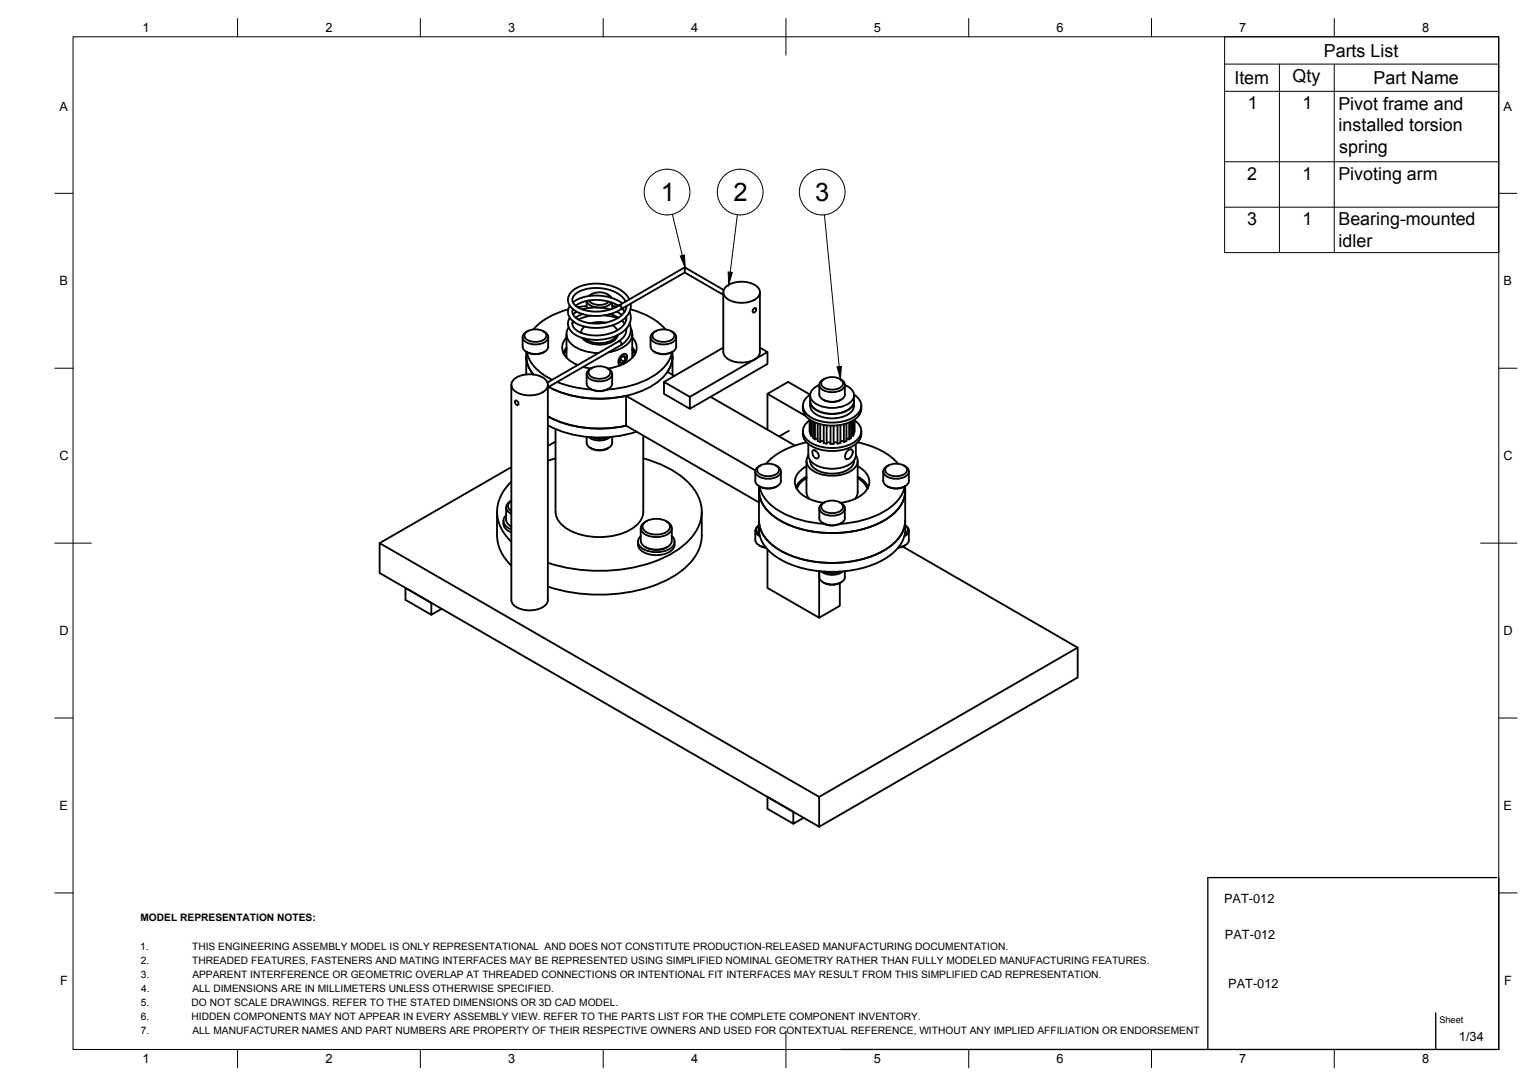
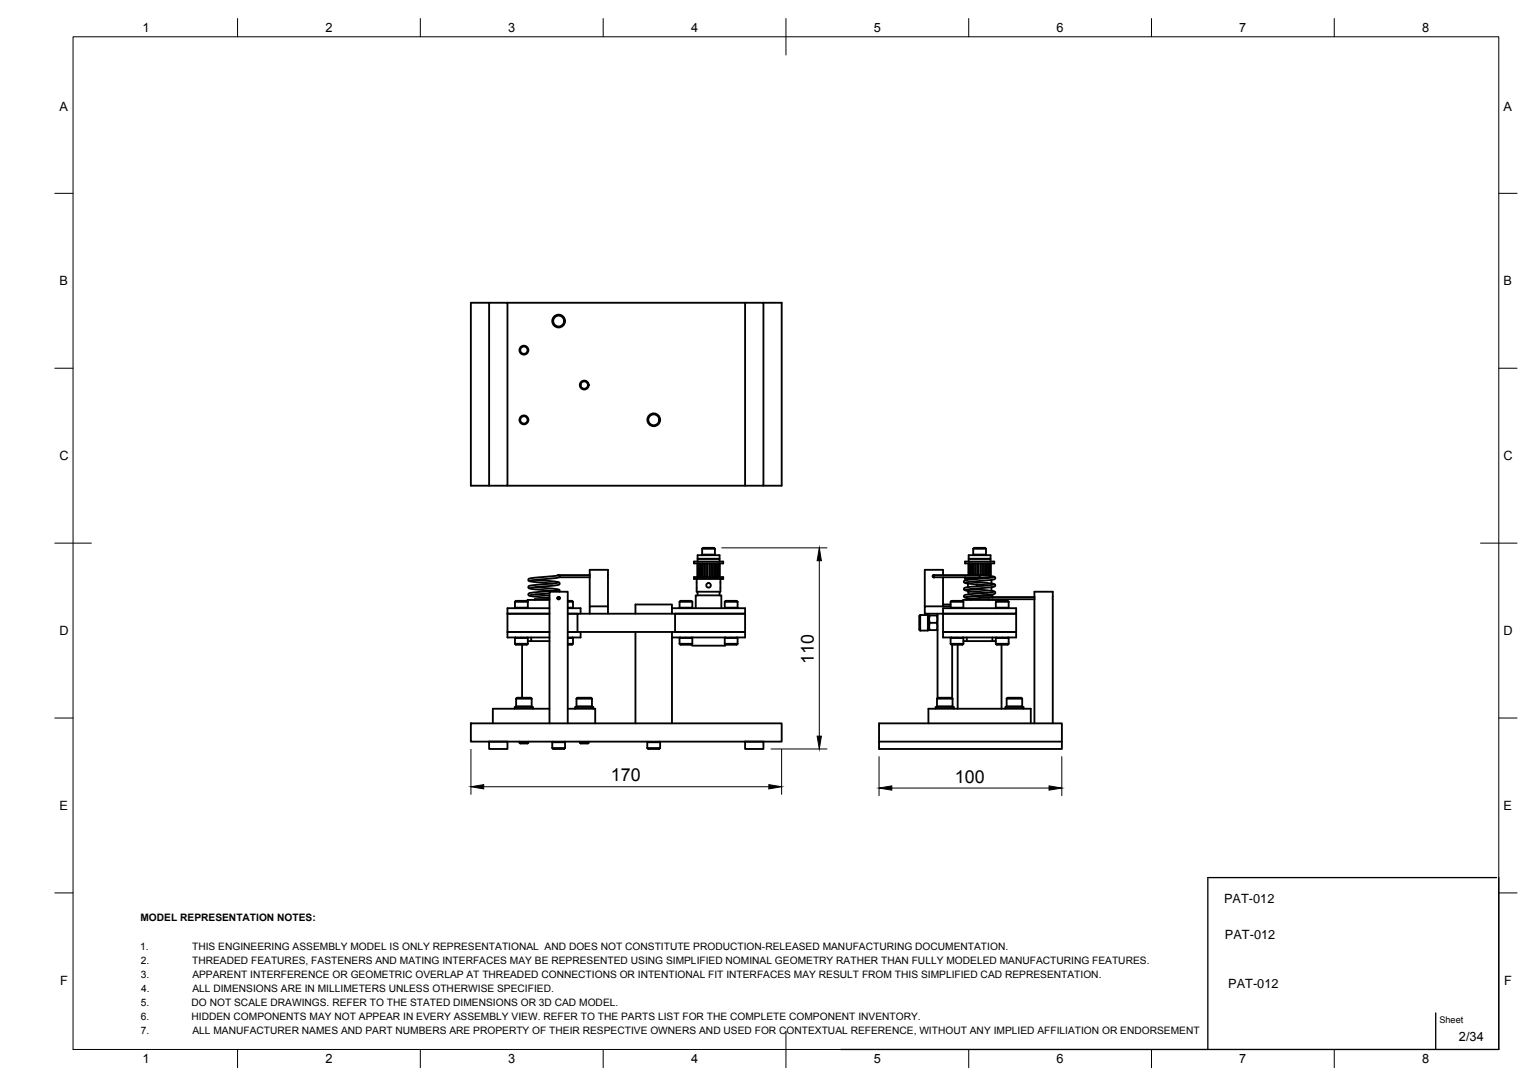
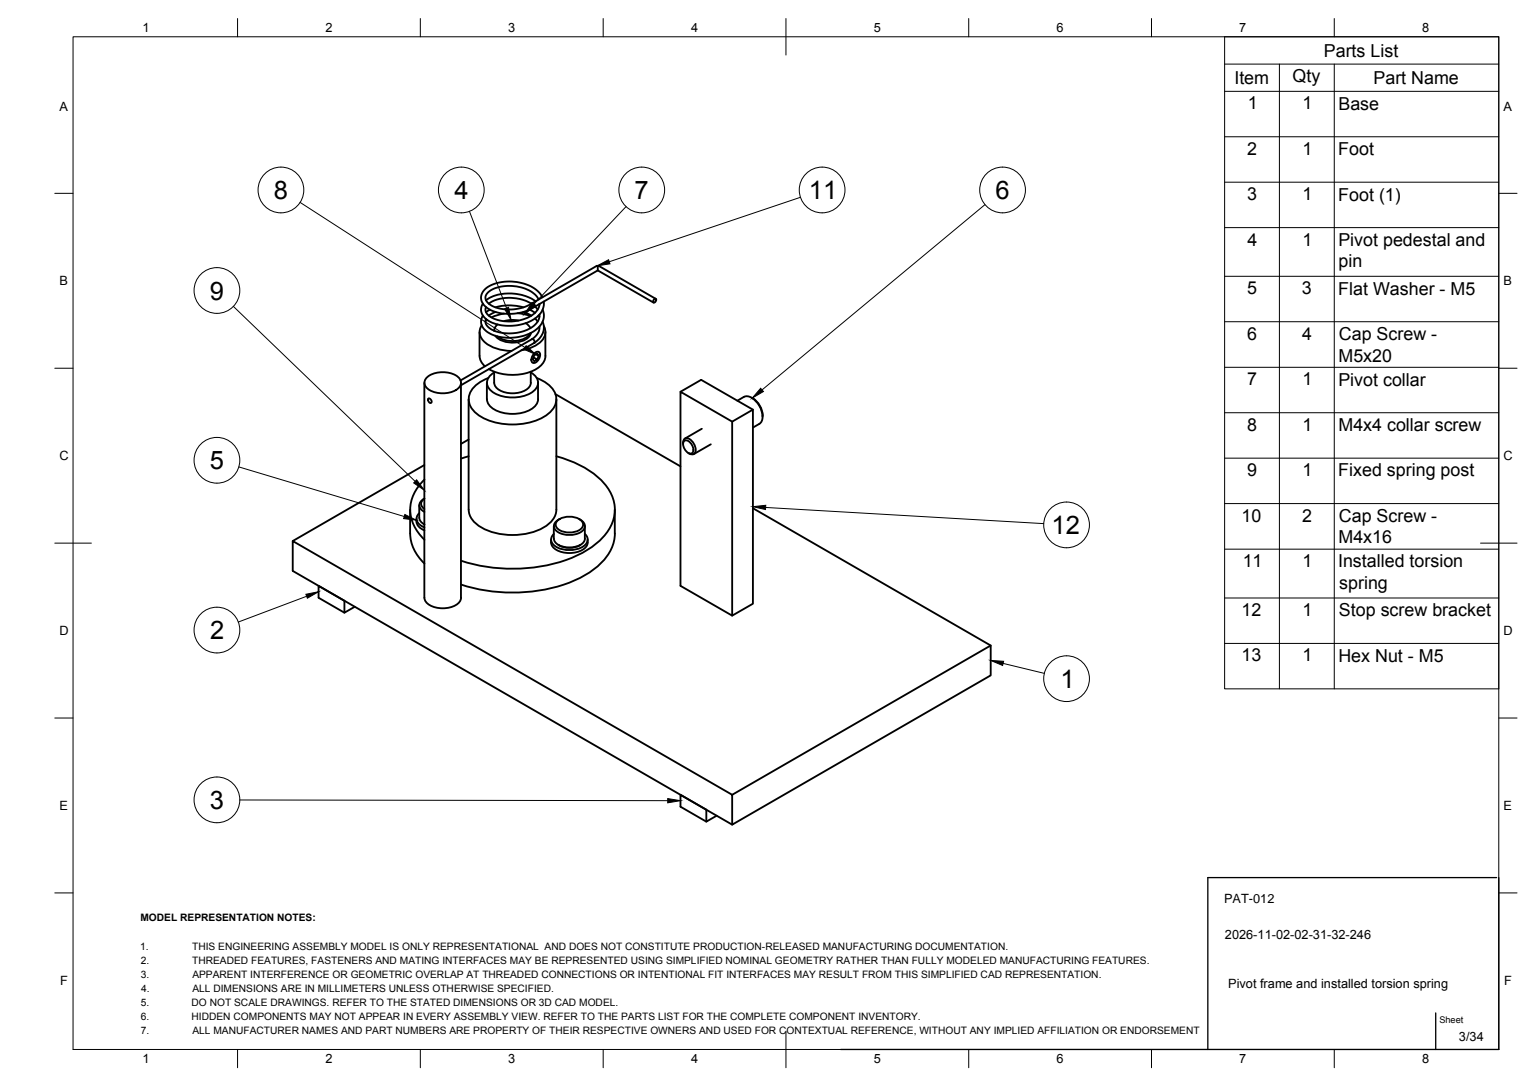
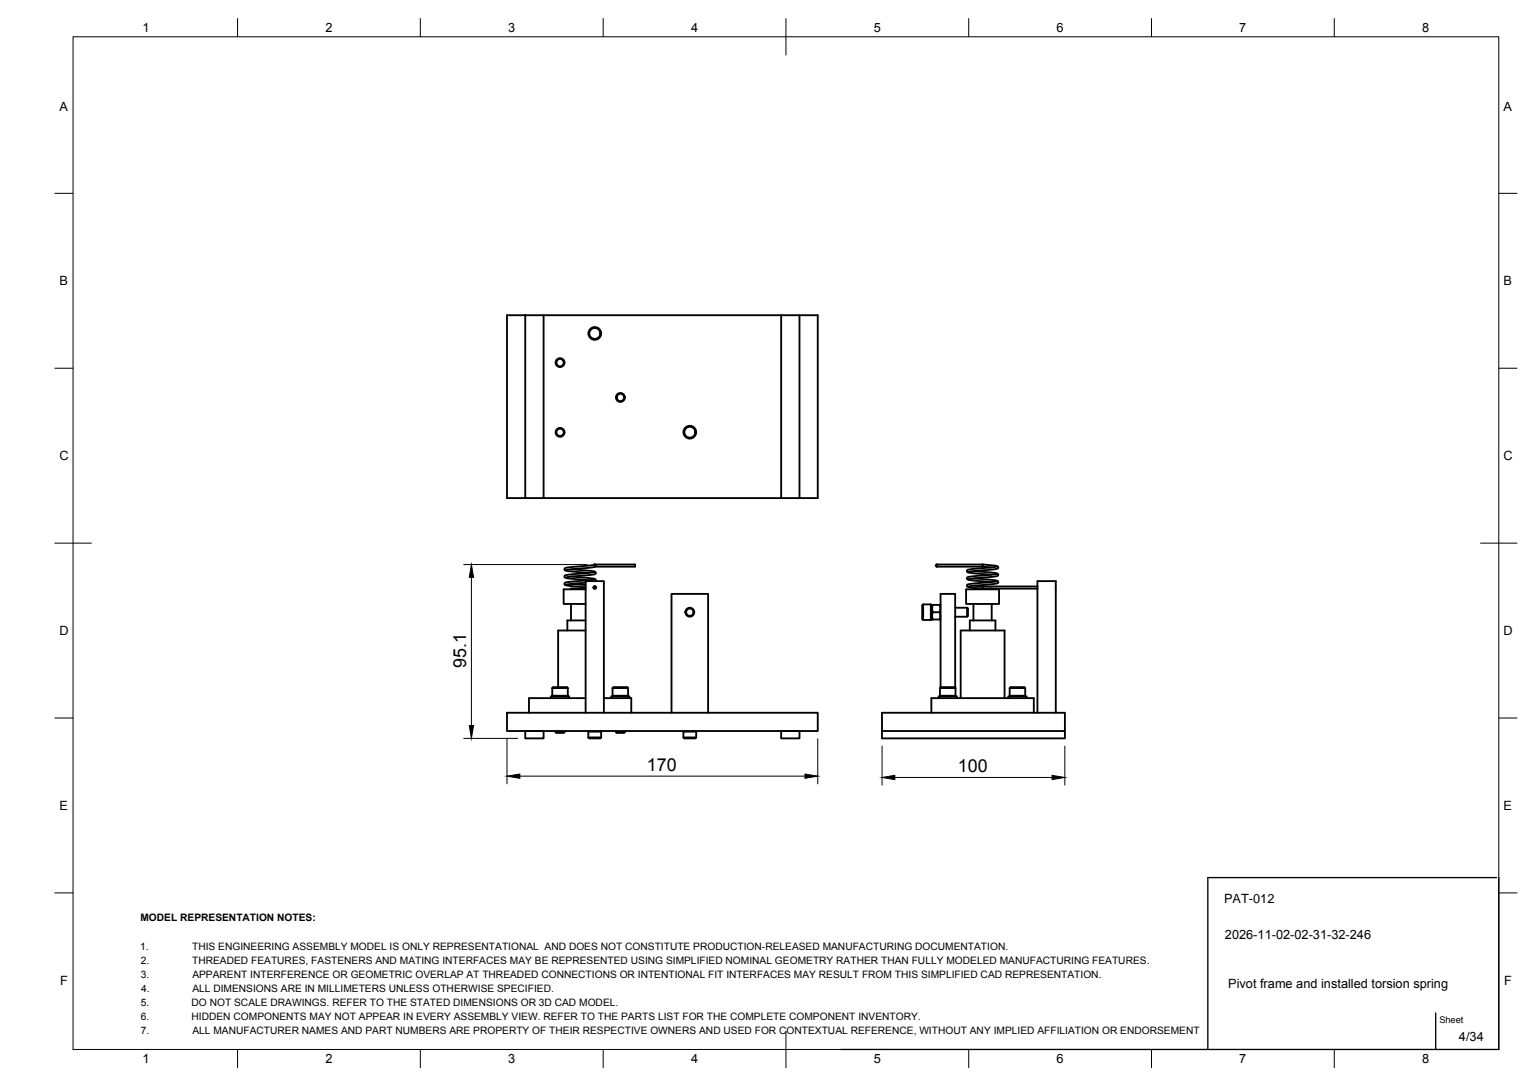
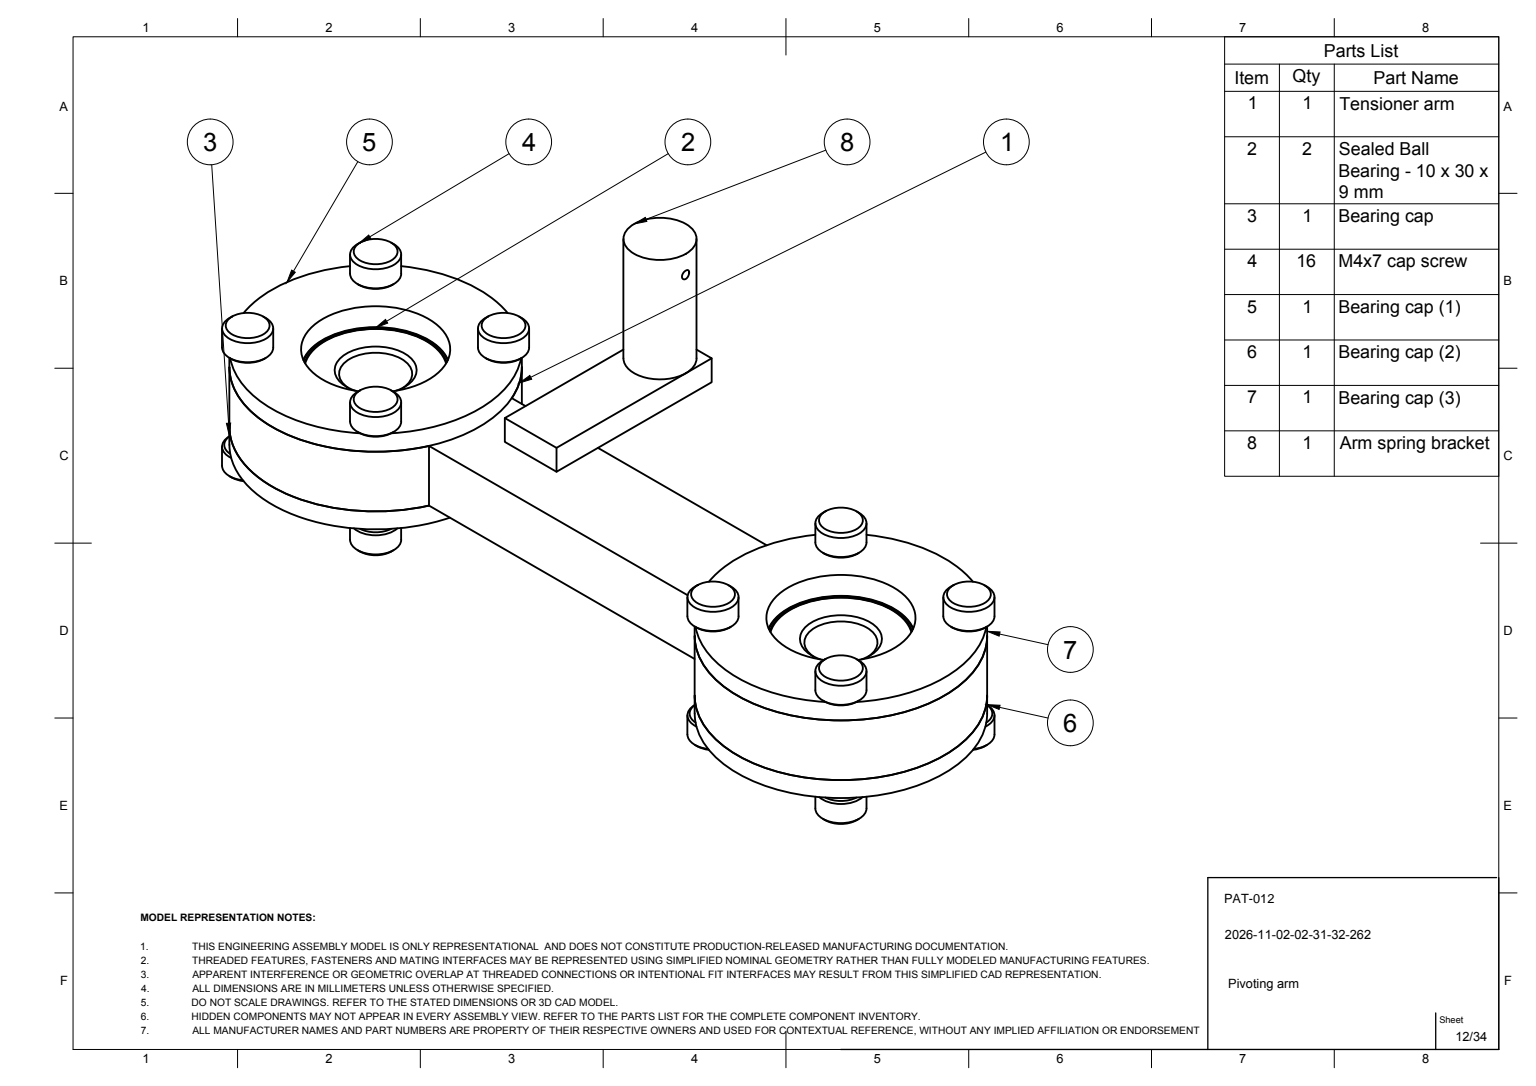
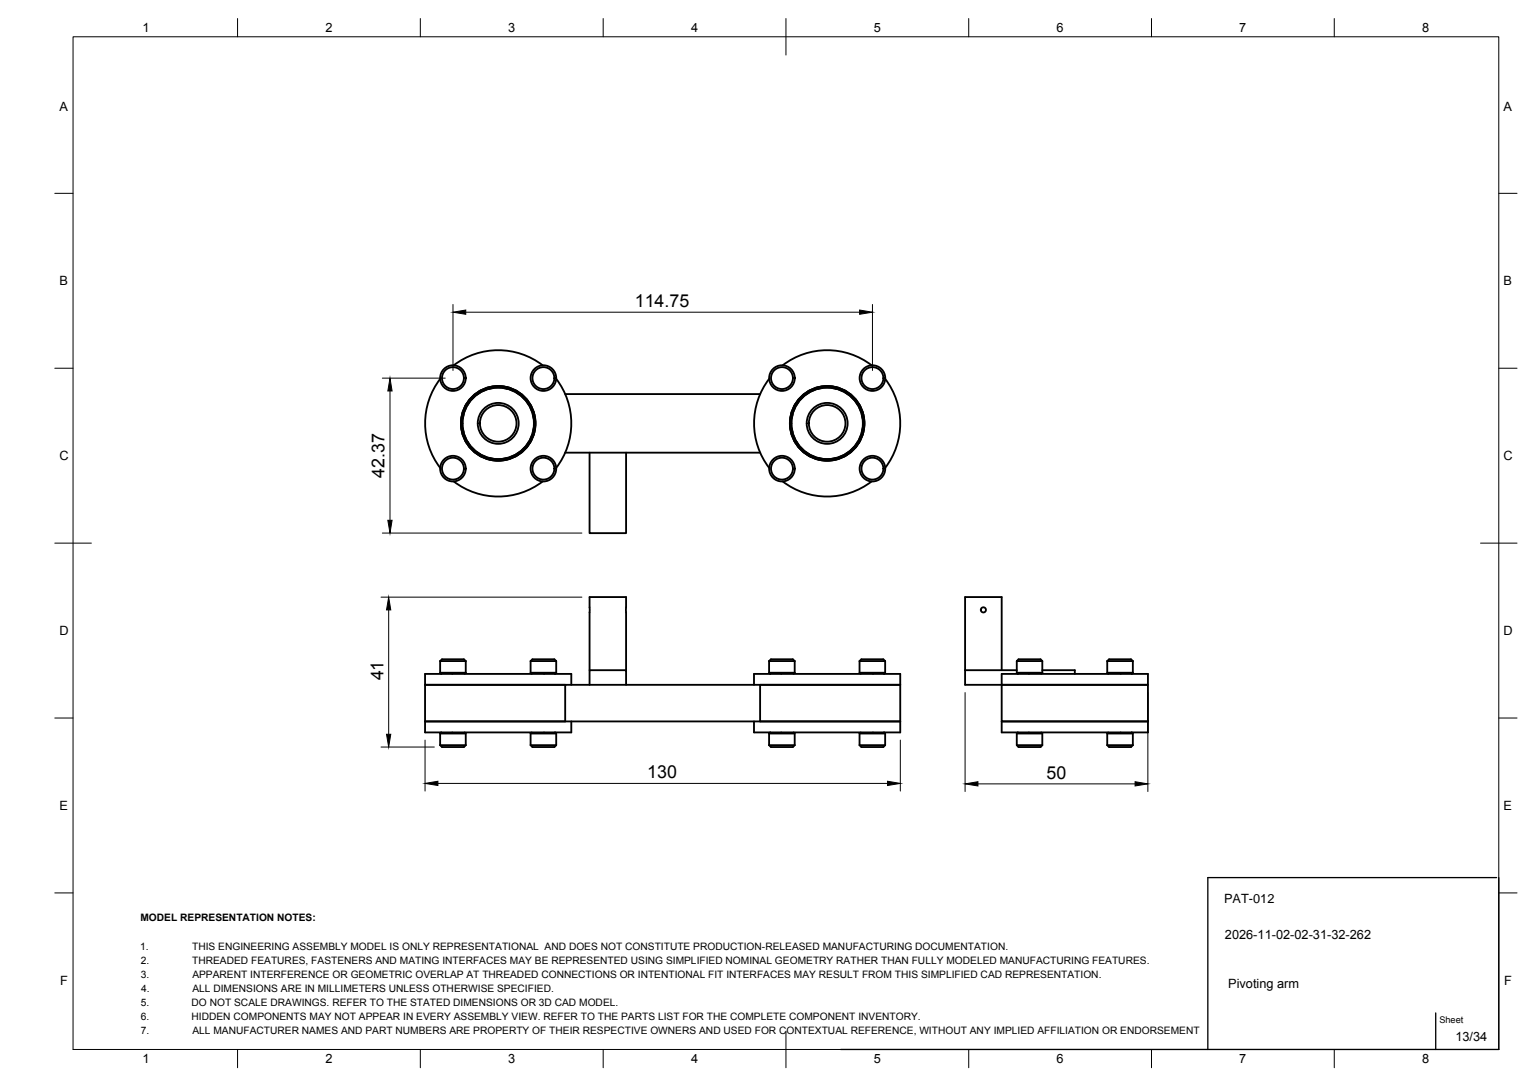
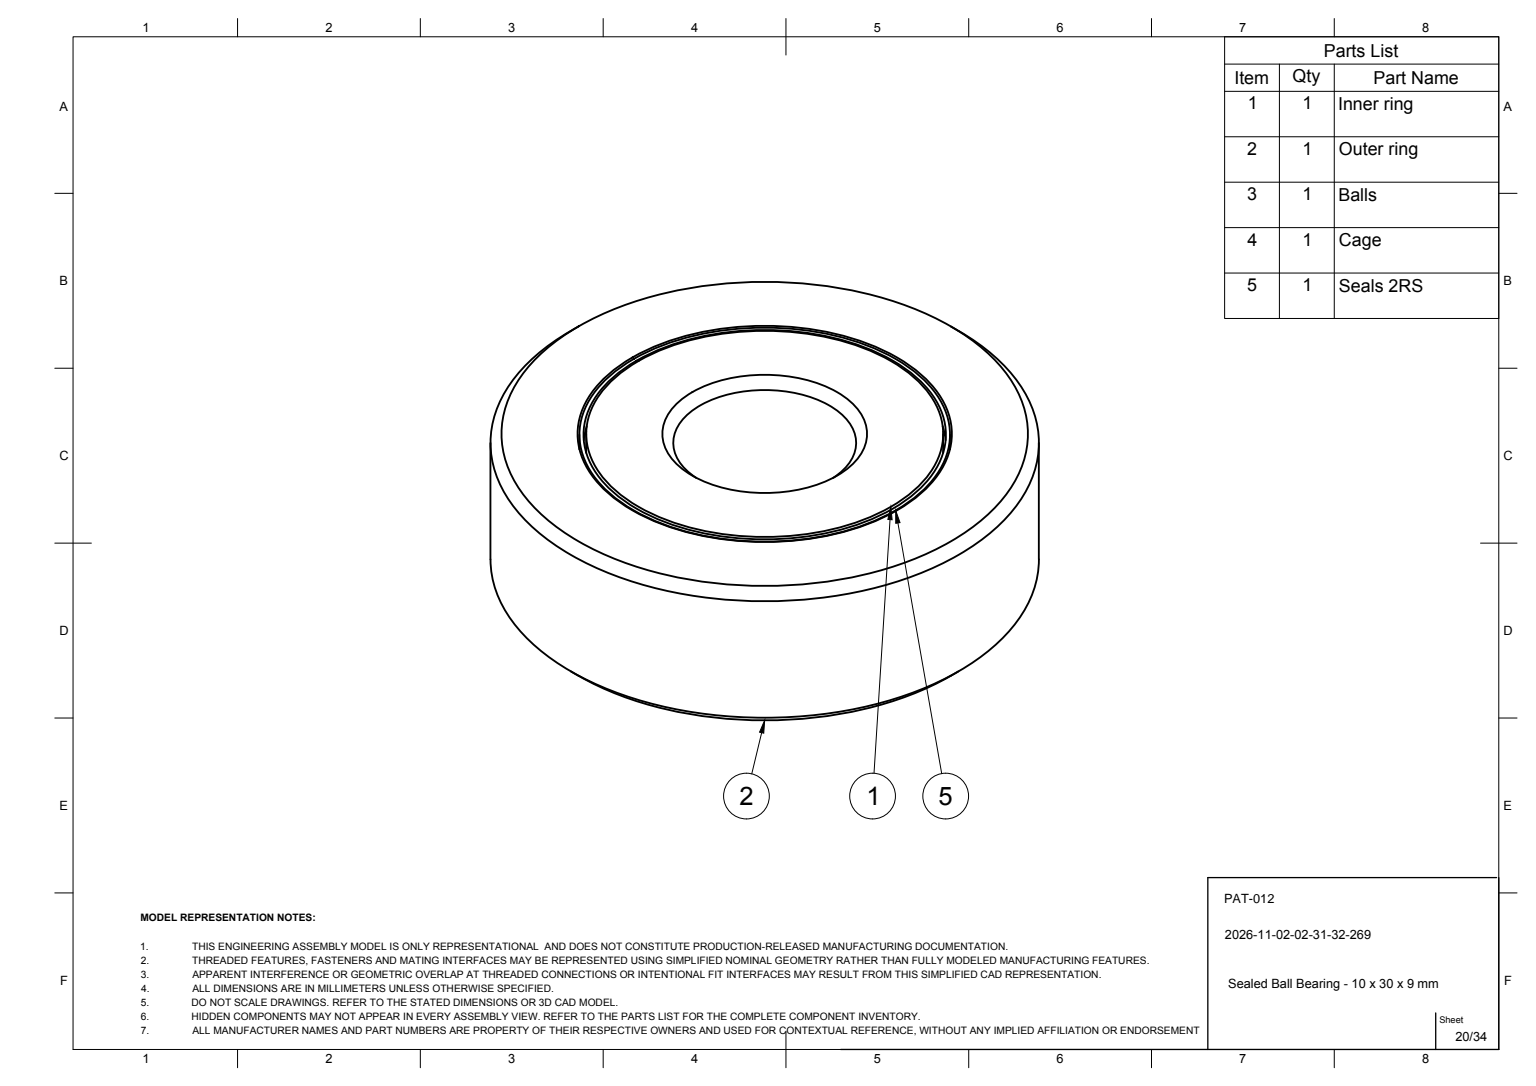
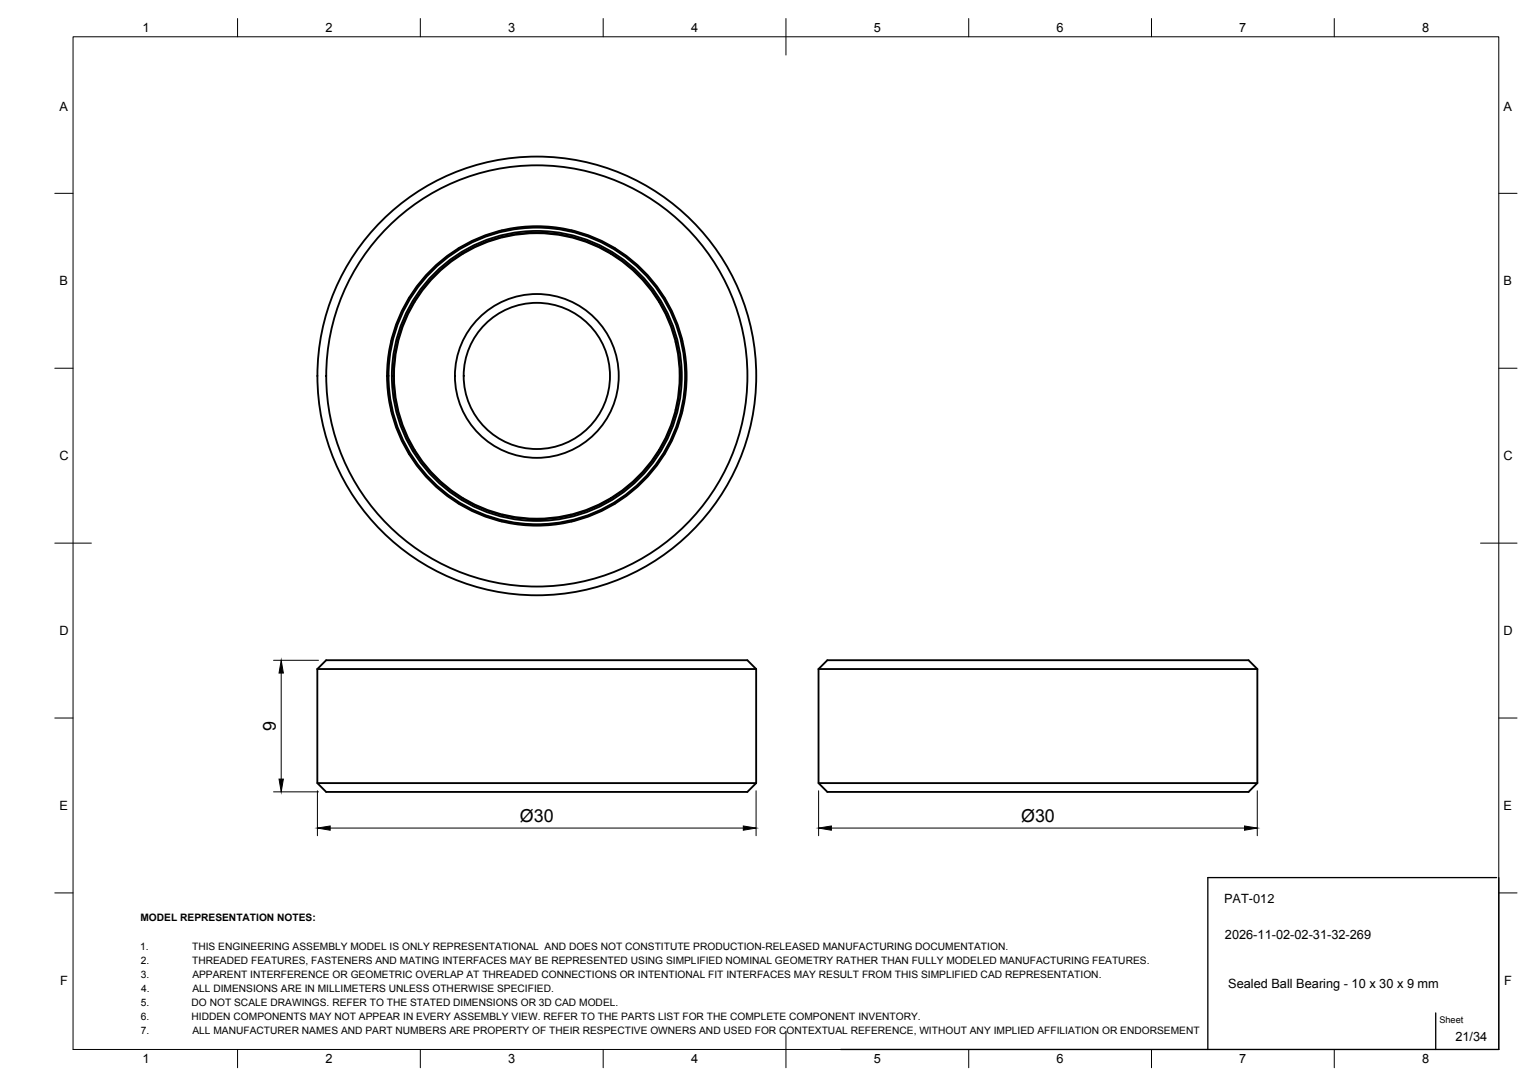
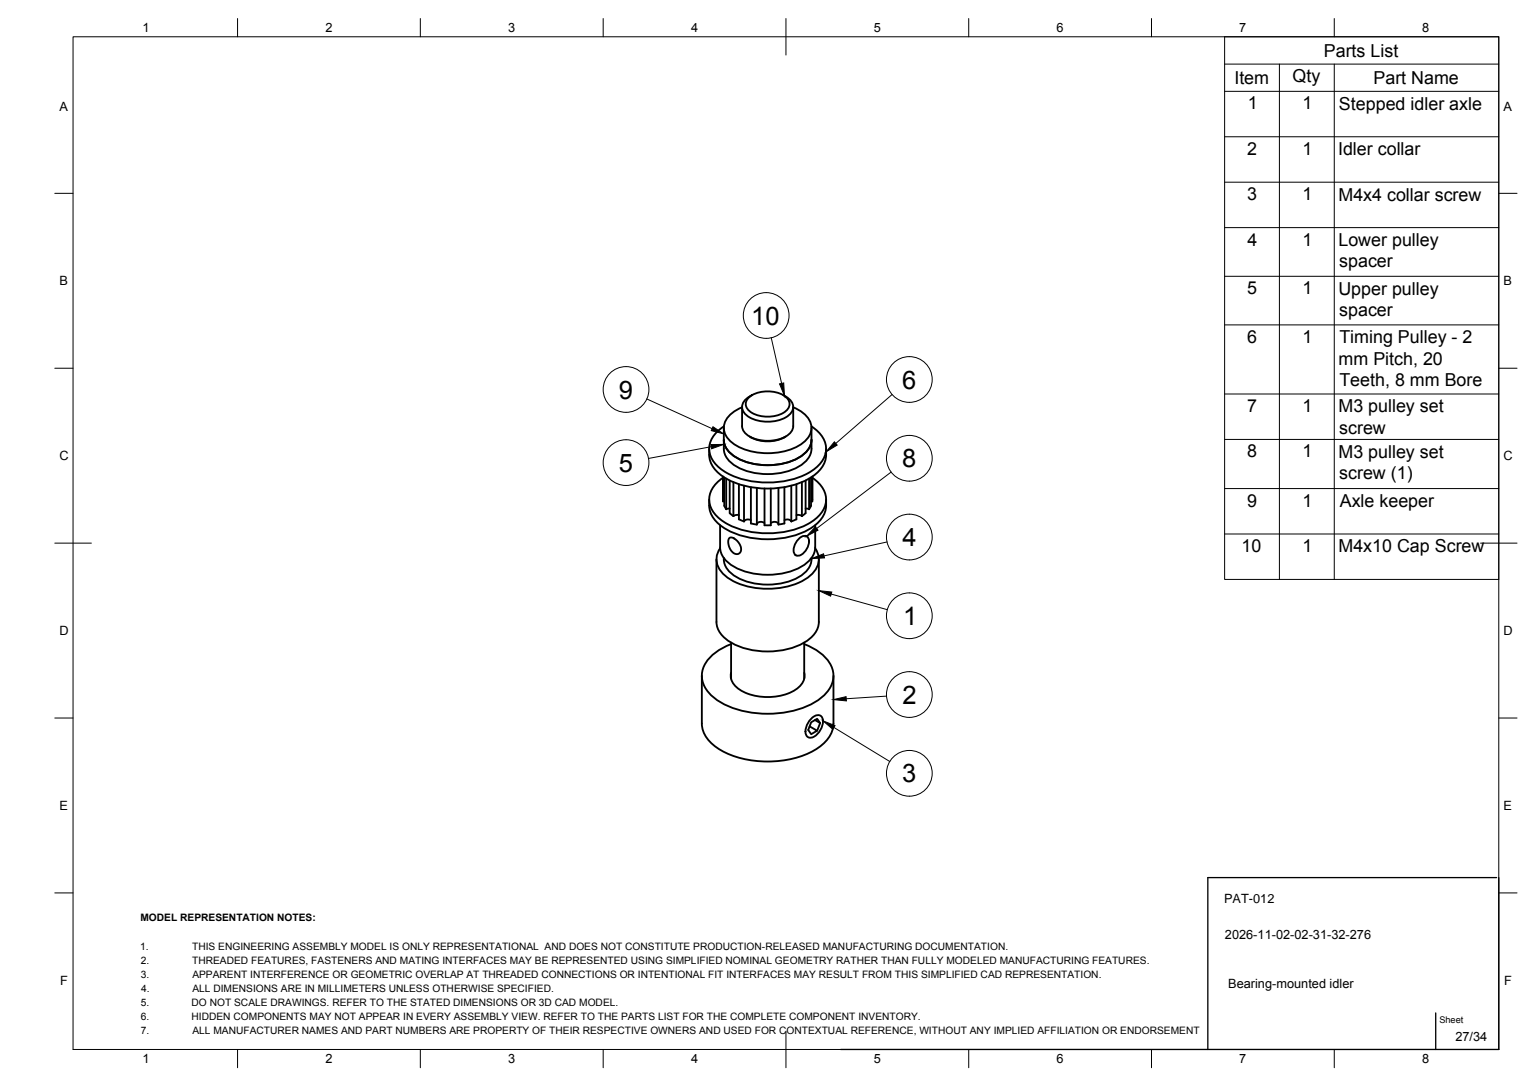
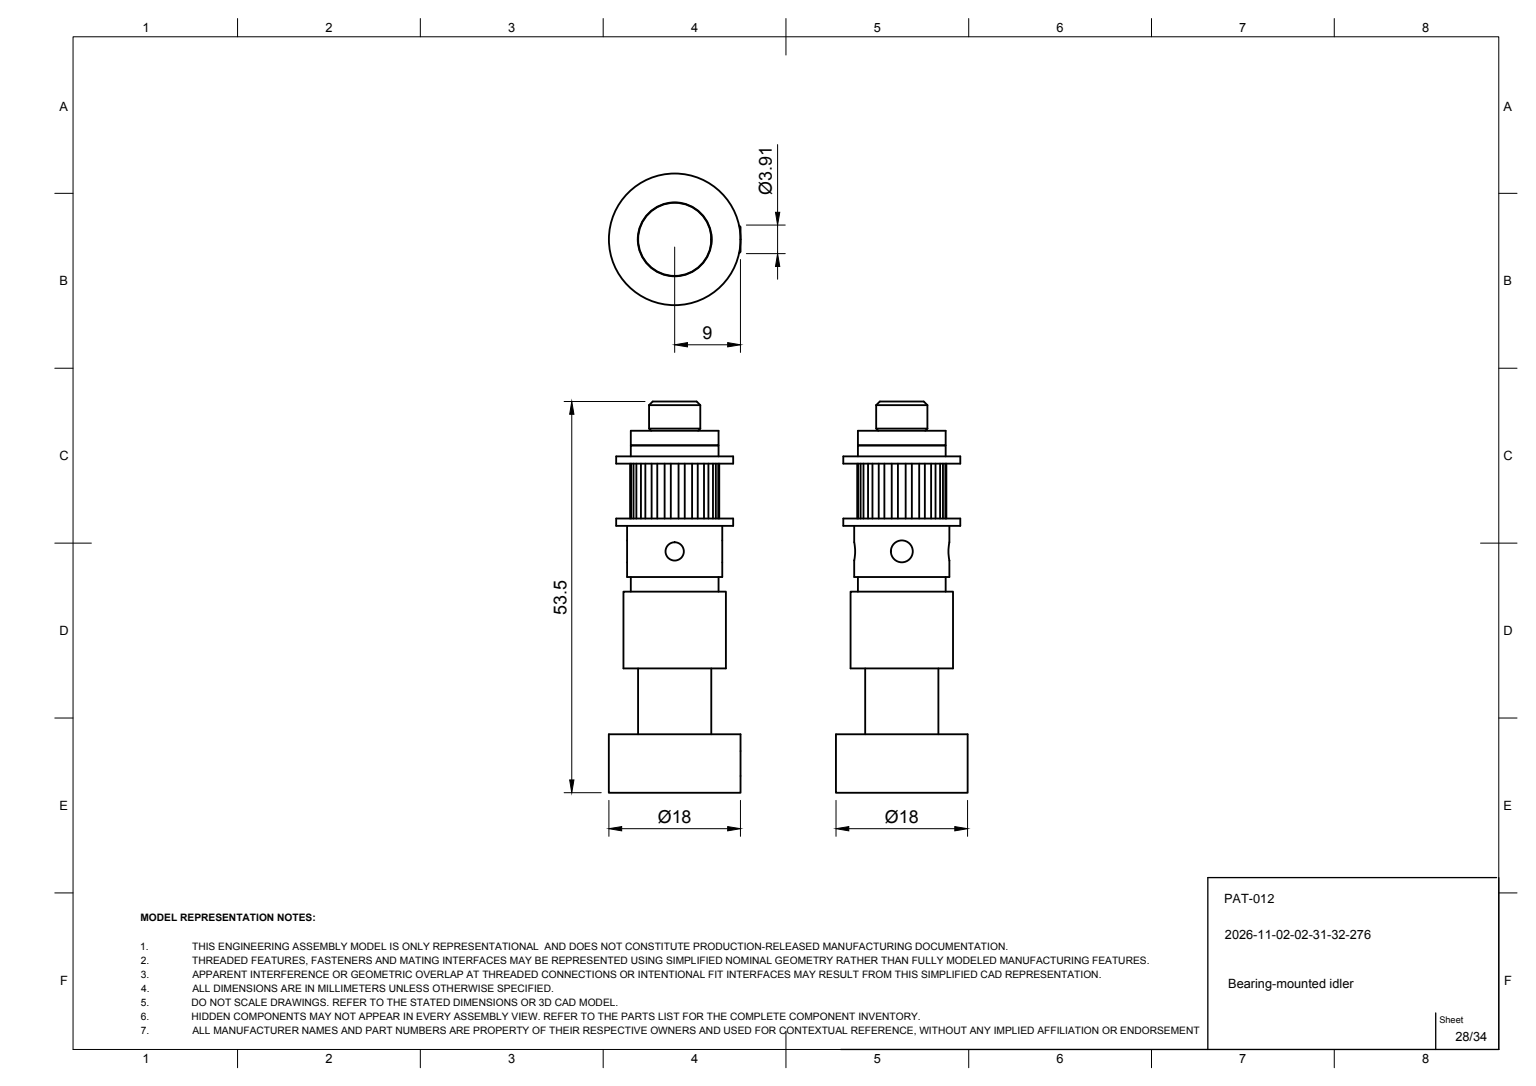
ISO-10303-21;
HEADER;
/* Generated by software containing ST-Developer
 * from STEP Tools, Inc. (www.steptools.com) 
 */

FILE_DESCRIPTION(
/* description */ ('Belt tensioner idler arm'),
/* implementation_level */ '2;1');

FILE_NAME(
/* name */ 'PAT-012',
/* time_stamp */ '2026-10-28T03:22:15-07:00',
/* author */ (''),
/* organization */ (''),
/* preprocessor_version */ 'ST-DEVELOPER v20.2',
/* originating_system */ 'Autodesk Translation Framework v15.17.0.0',
/* authorisation */ '');

FILE_SCHEMA (('AUTOMOTIVE_DESIGN { 1 0 10303 214 3 1 1 }'));
ENDSEC;

DATA;
#10=MECHANICAL_DESIGN_GEOMETRIC_PRESENTATION_REPRESENTATION('',(#447,#448,
#449,#450,#451,#452,#453,#454,#455,#456,#457,#458,#459,#460,#461,#462,#463,
#464,#465,#466,#467,#468,#469,#470,#471,#472,#473,#474,#475,#476,#477,#478,
#479,#480,#481,#482,#483,#484,#485,#486,#487,#488),#12779);
#11=ITEM_DEFINED_TRANSFORMATION($,$,#6967,#7095);
#12=ITEM_DEFINED_TRANSFORMATION($,$,#6987,#7096);
#13=ITEM_DEFINED_TRANSFORMATION($,$,#7007,#7097);
#14=ITEM_DEFINED_TRANSFORMATION($,$,#7024,#7098);
#15=ITEM_DEFINED_TRANSFORMATION($,$,#7078,#7099);
#16=ITEM_DEFINED_TRANSFORMATION($,$,#6809,#7124);
#17=ITEM_DEFINED_TRANSFORMATION($,$,#6850,#7125);
#18=ITEM_DEFINED_TRANSFORMATION($,$,#6875,#7126);
#19=ITEM_DEFINED_TRANSFORMATION($,$,#6900,#7127);
#20=ITEM_DEFINED_TRANSFORMATION($,$,#6925,#7128);
#21=ITEM_DEFINED_TRANSFORMATION($,$,#6950,#7129);
#22=ITEM_DEFINED_TRANSFORMATION($,$,#6966,#7130);
#23=ITEM_DEFINED_TRANSFORMATION($,$,#7100,#7131);
#24=ITEM_DEFINED_TRANSFORMATION($,$,#7100,#7132);
#25=ITEM_DEFINED_TRANSFORMATION($,$,#7100,#7133);
#26=ITEM_DEFINED_TRANSFORMATION($,$,#7100,#7134);
#27=ITEM_DEFINED_TRANSFORMATION($,$,#7100,#7135);
#28=ITEM_DEFINED_TRANSFORMATION($,$,#7100,#7136);
#29=ITEM_DEFINED_TRANSFORMATION($,$,#7100,#7137);
#30=ITEM_DEFINED_TRANSFORMATION($,$,#7100,#7138);
#31=ITEM_DEFINED_TRANSFORMATION($,$,#6966,#7139);
#32=ITEM_DEFINED_TRANSFORMATION($,$,#7100,#7140);
#33=ITEM_DEFINED_TRANSFORMATION($,$,#7100,#7141);
#34=ITEM_DEFINED_TRANSFORMATION($,$,#7100,#7142);
#35=ITEM_DEFINED_TRANSFORMATION($,$,#7100,#7143);
#36=ITEM_DEFINED_TRANSFORMATION($,$,#7100,#7144);
#37=ITEM_DEFINED_TRANSFORMATION($,$,#7100,#7145);
#38=ITEM_DEFINED_TRANSFORMATION($,$,#7100,#7146);
#39=ITEM_DEFINED_TRANSFORMATION($,$,#7100,#7147);
#40=ITEM_DEFINED_TRANSFORMATION($,$,#6604,#7235);
#41=ITEM_DEFINED_TRANSFORMATION($,$,#6626,#7236);
#42=ITEM_DEFINED_TRANSFORMATION($,$,#6633,#7237);
#43=ITEM_DEFINED_TRANSFORMATION($,$,#6640,#7238);
#44=ITEM_DEFINED_TRANSFORMATION($,$,#6667,#7239);
#45=ITEM_DEFINED_TRANSFORMATION($,$,#6681,#7240);
#46=ITEM_DEFINED_TRANSFORMATION($,$,#6692,#7241);
#47=ITEM_DEFINED_TRANSFORMATION($,$,#6715,#7242);
#48=ITEM_DEFINED_TRANSFORMATION($,$,#6729,#7243);
#49=ITEM_DEFINED_TRANSFORMATION($,$,#6740,#7244);
#50=ITEM_DEFINED_TRANSFORMATION($,$,#6729,#7245);
#51=ITEM_DEFINED_TRANSFORMATION($,$,#6740,#7246);
#52=ITEM_DEFINED_TRANSFORMATION($,$,#6729,#7247);
#53=ITEM_DEFINED_TRANSFORMATION($,$,#6740,#7248);
#54=ITEM_DEFINED_TRANSFORMATION($,$,#7220,#7249);
#55=ITEM_DEFINED_TRANSFORMATION($,$,#6782,#7250);
#56=ITEM_DEFINED_TRANSFORMATION($,$,#6740,#7251);
#57=ITEM_DEFINED_TRANSFORMATION($,$,#6766,#7252);
#58=ITEM_DEFINED_TRANSFORMATION($,$,#6782,#7253);
#59=ITEM_DEFINED_TRANSFORMATION($,$,#7149,#7420);
#60=ITEM_DEFINED_TRANSFORMATION($,$,#7167,#7421);
#61=ITEM_DEFINED_TRANSFORMATION($,$,#7181,#7422);
#62=ITEM_DEFINED_TRANSFORMATION($,$,#7190,#7423);
#63=ITEM_DEFINED_TRANSFORMATION($,$,#7199,#7424);
#64=ITEM_DEFINED_TRANSFORMATION($,$,#7205,#7425);
#65=ITEM_DEFINED_TRANSFORMATION($,$,#7211,#7426);
#66=ITEM_DEFINED_TRANSFORMATION($,$,#7220,#7427);
#67=ITEM_DEFINED_TRANSFORMATION($,$,#7254,#7428);
#68=ITEM_DEFINED_TRANSFORMATION($,$,#7396,#7429);
#69=ITEM_DEFINED_TRANSFORMATION($,$,#6603,#7430);
#70=ITEM_DEFINED_TRANSFORMATION($,$,#6808,#7431);
#71=ITEM_DEFINED_TRANSFORMATION($,$,#7148,#7432);
#72=(
REPRESENTATION_RELATIONSHIP($,$,#12945,#12944)
REPRESENTATION_RELATIONSHIP_WITH_TRANSFORMATION(#11)
SHAPE_REPRESENTATION_RELATIONSHIP()
);
#73=(
REPRESENTATION_RELATIONSHIP($,$,#12946,#12944)
REPRESENTATION_RELATIONSHIP_WITH_TRANSFORMATION(#12)
SHAPE_REPRESENTATION_RELATIONSHIP()
);
#74=(
REPRESENTATION_RELATIONSHIP($,$,#12947,#12944)
REPRESENTATION_RELATIONSHIP_WITH_TRANSFORMATION(#13)
SHAPE_REPRESENTATION_RELATIONSHIP()
);
#75=(
REPRESENTATION_RELATIONSHIP($,$,#12948,#12944)
REPRESENTATION_RELATIONSHIP_WITH_TRANSFORMATION(#14)
SHAPE_REPRESENTATION_RELATIONSHIP()
);
#76=(
REPRESENTATION_RELATIONSHIP($,$,#12949,#12944)
REPRESENTATION_RELATIONSHIP_WITH_TRANSFORMATION(#15)
SHAPE_REPRESENTATION_RELATIONSHIP()
);
#77=(
REPRESENTATION_RELATIONSHIP($,$,#12938,#12937)
REPRESENTATION_RELATIONSHIP_WITH_TRANSFORMATION(#16)
SHAPE_REPRESENTATION_RELATIONSHIP()
);
#78=(
REPRESENTATION_RELATIONSHIP($,$,#12939,#12937)
REPRESENTATION_RELATIONSHIP_WITH_TRANSFORMATION(#17)
SHAPE_REPRESENTATION_RELATIONSHIP()
);
#79=(
REPRESENTATION_RELATIONSHIP($,$,#12940,#12937)
REPRESENTATION_RELATIONSHIP_WITH_TRANSFORMATION(#18)
SHAPE_REPRESENTATION_RELATIONSHIP()
);
#80=(
REPRESENTATION_RELATIONSHIP($,$,#12941,#12937)
REPRESENTATION_RELATIONSHIP_WITH_TRANSFORMATION(#19)
SHAPE_REPRESENTATION_RELATIONSHIP()
);
#81=(
REPRESENTATION_RELATIONSHIP($,$,#12942,#12937)
REPRESENTATION_RELATIONSHIP_WITH_TRANSFORMATION(#20)
SHAPE_REPRESENTATION_RELATIONSHIP()
);
#82=(
REPRESENTATION_RELATIONSHIP($,$,#12943,#12937)
REPRESENTATION_RELATIONSHIP_WITH_TRANSFORMATION(#21)
SHAPE_REPRESENTATION_RELATIONSHIP()
);
#83=(
REPRESENTATION_RELATIONSHIP($,$,#12944,#12937)
REPRESENTATION_RELATIONSHIP_WITH_TRANSFORMATION(#22)
SHAPE_REPRESENTATION_RELATIONSHIP()
);
#84=(
REPRESENTATION_RELATIONSHIP($,$,#12950,#12937)
REPRESENTATION_RELATIONSHIP_WITH_TRANSFORMATION(#23)
SHAPE_REPRESENTATION_RELATIONSHIP()
);
#85=(
REPRESENTATION_RELATIONSHIP($,$,#12950,#12937)
REPRESENTATION_RELATIONSHIP_WITH_TRANSFORMATION(#24)
SHAPE_REPRESENTATION_RELATIONSHIP()
);
#86=(
REPRESENTATION_RELATIONSHIP($,$,#12950,#12937)
REPRESENTATION_RELATIONSHIP_WITH_TRANSFORMATION(#25)
SHAPE_REPRESENTATION_RELATIONSHIP()
);
#87=(
REPRESENTATION_RELATIONSHIP($,$,#12950,#12937)
REPRESENTATION_RELATIONSHIP_WITH_TRANSFORMATION(#26)
SHAPE_REPRESENTATION_RELATIONSHIP()
);
#88=(
REPRESENTATION_RELATIONSHIP($,$,#12950,#12937)
REPRESENTATION_RELATIONSHIP_WITH_TRANSFORMATION(#27)
SHAPE_REPRESENTATION_RELATIONSHIP()
);
#89=(
REPRESENTATION_RELATIONSHIP($,$,#12950,#12937)
REPRESENTATION_RELATIONSHIP_WITH_TRANSFORMATION(#28)
SHAPE_REPRESENTATION_RELATIONSHIP()
);
#90=(
REPRESENTATION_RELATIONSHIP($,$,#12950,#12937)
REPRESENTATION_RELATIONSHIP_WITH_TRANSFORMATION(#29)
SHAPE_REPRESENTATION_RELATIONSHIP()
);
#91=(
REPRESENTATION_RELATIONSHIP($,$,#12950,#12937)
REPRESENTATION_RELATIONSHIP_WITH_TRANSFORMATION(#30)
SHAPE_REPRESENTATION_RELATIONSHIP()
);
#92=(
REPRESENTATION_RELATIONSHIP($,$,#12944,#12937)
REPRESENTATION_RELATIONSHIP_WITH_TRANSFORMATION(#31)
SHAPE_REPRESENTATION_RELATIONSHIP()
);
#93=(
REPRESENTATION_RELATIONSHIP($,$,#12950,#12937)
REPRESENTATION_RELATIONSHIP_WITH_TRANSFORMATION(#32)
SHAPE_REPRESENTATION_RELATIONSHIP()
);
#94=(
REPRESENTATION_RELATIONSHIP($,$,#12950,#12937)
REPRESENTATION_RELATIONSHIP_WITH_TRANSFORMATION(#33)
SHAPE_REPRESENTATION_RELATIONSHIP()
);
#95=(
REPRESENTATION_RELATIONSHIP($,$,#12950,#12937)
REPRESENTATION_RELATIONSHIP_WITH_TRANSFORMATION(#34)
SHAPE_REPRESENTATION_RELATIONSHIP()
);
#96=(
REPRESENTATION_RELATIONSHIP($,$,#12950,#12937)
REPRESENTATION_RELATIONSHIP_WITH_TRANSFORMATION(#35)
SHAPE_REPRESENTATION_RELATIONSHIP()
);
#97=(
REPRESENTATION_RELATIONSHIP($,$,#12950,#12937)
REPRESENTATION_RELATIONSHIP_WITH_TRANSFORMATION(#36)
SHAPE_REPRESENTATION_RELATIONSHIP()
);
#98=(
REPRESENTATION_RELATIONSHIP($,$,#12950,#12937)
REPRESENTATION_RELATIONSHIP_WITH_TRANSFORMATION(#37)
SHAPE_REPRESENTATION_RELATIONSHIP()
);
#99=(
REPRESENTATION_RELATIONSHIP($,$,#12950,#12937)
REPRESENTATION_RELATIONSHIP_WITH_TRANSFORMATION(#38)
SHAPE_REPRESENTATION_RELATIONSHIP()
);
#100=(
REPRESENTATION_RELATIONSHIP($,$,#12950,#12937)
REPRESENTATION_RELATIONSHIP_WITH_TRANSFORMATION(#39)
SHAPE_REPRESENTATION_RELATIONSHIP()
);
#101=(
REPRESENTATION_RELATIONSHIP($,$,#12925,#12924)
REPRESENTATION_RELATIONSHIP_WITH_TRANSFORMATION(#40)
SHAPE_REPRESENTATION_RELATIONSHIP()
);
#102=(
REPRESENTATION_RELATIONSHIP($,$,#12926,#12924)
REPRESENTATION_RELATIONSHIP_WITH_TRANSFORMATION(#41)
SHAPE_REPRESENTATION_RELATIONSHIP()
);
#103=(
REPRESENTATION_RELATIONSHIP($,$,#12927,#12924)
REPRESENTATION_RELATIONSHIP_WITH_TRANSFORMATION(#42)
SHAPE_REPRESENTATION_RELATIONSHIP()
);
#104=(
REPRESENTATION_RELATIONSHIP($,$,#12928,#12924)
REPRESENTATION_RELATIONSHIP_WITH_TRANSFORMATION(#43)
SHAPE_REPRESENTATION_RELATIONSHIP()
);
#105=(
REPRESENTATION_RELATIONSHIP($,$,#12929,#12924)
REPRESENTATION_RELATIONSHIP_WITH_TRANSFORMATION(#44)
SHAPE_REPRESENTATION_RELATIONSHIP()
);
#106=(
REPRESENTATION_RELATIONSHIP($,$,#12930,#12924)
REPRESENTATION_RELATIONSHIP_WITH_TRANSFORMATION(#45)
SHAPE_REPRESENTATION_RELATIONSHIP()
);
#107=(
REPRESENTATION_RELATIONSHIP($,$,#12931,#12924)
REPRESENTATION_RELATIONSHIP_WITH_TRANSFORMATION(#46)
SHAPE_REPRESENTATION_RELATIONSHIP()
);
#108=(
REPRESENTATION_RELATIONSHIP($,$,#12932,#12924)
REPRESENTATION_RELATIONSHIP_WITH_TRANSFORMATION(#47)
SHAPE_REPRESENTATION_RELATIONSHIP()
);
#109=(
REPRESENTATION_RELATIONSHIP($,$,#12933,#12924)
REPRESENTATION_RELATIONSHIP_WITH_TRANSFORMATION(#48)
SHAPE_REPRESENTATION_RELATIONSHIP()
);
#110=(
REPRESENTATION_RELATIONSHIP($,$,#12934,#12924)
REPRESENTATION_RELATIONSHIP_WITH_TRANSFORMATION(#49)
SHAPE_REPRESENTATION_RELATIONSHIP()
);
#111=(
REPRESENTATION_RELATIONSHIP($,$,#12933,#12924)
REPRESENTATION_RELATIONSHIP_WITH_TRANSFORMATION(#50)
SHAPE_REPRESENTATION_RELATIONSHIP()
);
#112=(
REPRESENTATION_RELATIONSHIP($,$,#12934,#12924)
REPRESENTATION_RELATIONSHIP_WITH_TRANSFORMATION(#51)
SHAPE_REPRESENTATION_RELATIONSHIP()
);
#113=(
REPRESENTATION_RELATIONSHIP($,$,#12933,#12924)
REPRESENTATION_RELATIONSHIP_WITH_TRANSFORMATION(#52)
SHAPE_REPRESENTATION_RELATIONSHIP()
);
#114=(
REPRESENTATION_RELATIONSHIP($,$,#12934,#12924)
REPRESENTATION_RELATIONSHIP_WITH_TRANSFORMATION(#53)
SHAPE_REPRESENTATION_RELATIONSHIP()
);
#115=(
REPRESENTATION_RELATIONSHIP($,$,#12959,#12924)
REPRESENTATION_RELATIONSHIP_WITH_TRANSFORMATION(#54)
SHAPE_REPRESENTATION_RELATIONSHIP()
);
#116=(
REPRESENTATION_RELATIONSHIP($,$,#12936,#12924)
REPRESENTATION_RELATIONSHIP_WITH_TRANSFORMATION(#55)
SHAPE_REPRESENTATION_RELATIONSHIP()
);
#117=(
REPRESENTATION_RELATIONSHIP($,$,#12934,#12924)
REPRESENTATION_RELATIONSHIP_WITH_TRANSFORMATION(#56)
SHAPE_REPRESENTATION_RELATIONSHIP()
);
#118=(
REPRESENTATION_RELATIONSHIP($,$,#12935,#12924)
REPRESENTATION_RELATIONSHIP_WITH_TRANSFORMATION(#57)
SHAPE_REPRESENTATION_RELATIONSHIP()
);
#119=(
REPRESENTATION_RELATIONSHIP($,$,#12936,#12924)
REPRESENTATION_RELATIONSHIP_WITH_TRANSFORMATION(#58)
SHAPE_REPRESENTATION_RELATIONSHIP()
);
#120=(
REPRESENTATION_RELATIONSHIP($,$,#12952,#12951)
REPRESENTATION_RELATIONSHIP_WITH_TRANSFORMATION(#59)
SHAPE_REPRESENTATION_RELATIONSHIP()
);
#121=(
REPRESENTATION_RELATIONSHIP($,$,#12953,#12951)
REPRESENTATION_RELATIONSHIP_WITH_TRANSFORMATION(#60)
SHAPE_REPRESENTATION_RELATIONSHIP()
);
#122=(
REPRESENTATION_RELATIONSHIP($,$,#12954,#12951)
REPRESENTATION_RELATIONSHIP_WITH_TRANSFORMATION(#61)
SHAPE_REPRESENTATION_RELATIONSHIP()
);
#123=(
REPRESENTATION_RELATIONSHIP($,$,#12955,#12951)
REPRESENTATION_RELATIONSHIP_WITH_TRANSFORMATION(#62)
SHAPE_REPRESENTATION_RELATIONSHIP()
);
#124=(
REPRESENTATION_RELATIONSHIP($,$,#12956,#12951)
REPRESENTATION_RELATIONSHIP_WITH_TRANSFORMATION(#63)
SHAPE_REPRESENTATION_RELATIONSHIP()
);
#125=(
REPRESENTATION_RELATIONSHIP($,$,#12957,#12951)
REPRESENTATION_RELATIONSHIP_WITH_TRANSFORMATION(#64)
SHAPE_REPRESENTATION_RELATIONSHIP()
);
#126=(
REPRESENTATION_RELATIONSHIP($,$,#12958,#12951)
REPRESENTATION_RELATIONSHIP_WITH_TRANSFORMATION(#65)
SHAPE_REPRESENTATION_RELATIONSHIP()
);
#127=(
REPRESENTATION_RELATIONSHIP($,$,#12959,#12951)
REPRESENTATION_RELATIONSHIP_WITH_TRANSFORMATION(#66)
SHAPE_REPRESENTATION_RELATIONSHIP()
);
#128=(
REPRESENTATION_RELATIONSHIP($,$,#12960,#12951)
REPRESENTATION_RELATIONSHIP_WITH_TRANSFORMATION(#67)
SHAPE_REPRESENTATION_RELATIONSHIP()
);
#129=(
REPRESENTATION_RELATIONSHIP($,$,#12961,#12951)
REPRESENTATION_RELATIONSHIP_WITH_TRANSFORMATION(#68)
SHAPE_REPRESENTATION_RELATIONSHIP()
);
#130=(
REPRESENTATION_RELATIONSHIP($,$,#12924,#12923)
REPRESENTATION_RELATIONSHIP_WITH_TRANSFORMATION(#69)
SHAPE_REPRESENTATION_RELATIONSHIP()
);
#131=(
REPRESENTATION_RELATIONSHIP($,$,#12937,#12923)
REPRESENTATION_RELATIONSHIP_WITH_TRANSFORMATION(#70)
SHAPE_REPRESENTATION_RELATIONSHIP()
);
#132=(
REPRESENTATION_RELATIONSHIP($,$,#12951,#12923)
REPRESENTATION_RELATIONSHIP_WITH_TRANSFORMATION(#71)
SHAPE_REPRESENTATION_RELATIONSHIP()
);
#133=CONTEXT_DEPENDENT_SHAPE_REPRESENTATION(#72,#12850);
#134=CONTEXT_DEPENDENT_SHAPE_REPRESENTATION(#73,#12851);
#135=CONTEXT_DEPENDENT_SHAPE_REPRESENTATION(#74,#12852);
#136=CONTEXT_DEPENDENT_SHAPE_REPRESENTATION(#75,#12853);
#137=CONTEXT_DEPENDENT_SHAPE_REPRESENTATION(#76,#12854);
#138=CONTEXT_DEPENDENT_SHAPE_REPRESENTATION(#77,#12856);
#139=CONTEXT_DEPENDENT_SHAPE_REPRESENTATION(#78,#12857);
#140=CONTEXT_DEPENDENT_SHAPE_REPRESENTATION(#79,#12858);
#141=CONTEXT_DEPENDENT_SHAPE_REPRESENTATION(#80,#12859);
#142=CONTEXT_DEPENDENT_SHAPE_REPRESENTATION(#81,#12860);
#143=CONTEXT_DEPENDENT_SHAPE_REPRESENTATION(#82,#12861);
#144=CONTEXT_DEPENDENT_SHAPE_REPRESENTATION(#83,#12862);
#145=CONTEXT_DEPENDENT_SHAPE_REPRESENTATION(#84,#12863);
#146=CONTEXT_DEPENDENT_SHAPE_REPRESENTATION(#85,#12864);
#147=CONTEXT_DEPENDENT_SHAPE_REPRESENTATION(#86,#12865);
#148=CONTEXT_DEPENDENT_SHAPE_REPRESENTATION(#87,#12866);
#149=CONTEXT_DEPENDENT_SHAPE_REPRESENTATION(#88,#12867);
#150=CONTEXT_DEPENDENT_SHAPE_REPRESENTATION(#89,#12868);
#151=CONTEXT_DEPENDENT_SHAPE_REPRESENTATION(#90,#12869);
#152=CONTEXT_DEPENDENT_SHAPE_REPRESENTATION(#91,#12870);
#153=CONTEXT_DEPENDENT_SHAPE_REPRESENTATION(#92,#12871);
#154=CONTEXT_DEPENDENT_SHAPE_REPRESENTATION(#93,#12872);
#155=CONTEXT_DEPENDENT_SHAPE_REPRESENTATION(#94,#12873);
#156=CONTEXT_DEPENDENT_SHAPE_REPRESENTATION(#95,#12874);
#157=CONTEXT_DEPENDENT_SHAPE_REPRESENTATION(#96,#12875);
#158=CONTEXT_DEPENDENT_SHAPE_REPRESENTATION(#97,#12876);
#159=CONTEXT_DEPENDENT_SHAPE_REPRESENTATION(#98,#12877);
#160=CONTEXT_DEPENDENT_SHAPE_REPRESENTATION(#99,#12878);
#161=CONTEXT_DEPENDENT_SHAPE_REPRESENTATION(#100,#12879);
#162=CONTEXT_DEPENDENT_SHAPE_REPRESENTATION(#101,#12889);
#163=CONTEXT_DEPENDENT_SHAPE_REPRESENTATION(#102,#12890);
#164=CONTEXT_DEPENDENT_SHAPE_REPRESENTATION(#103,#12891);
#165=CONTEXT_DEPENDENT_SHAPE_REPRESENTATION(#104,#12892);
#166=CONTEXT_DEPENDENT_SHAPE_REPRESENTATION(#105,#12893);
#167=CONTEXT_DEPENDENT_SHAPE_REPRESENTATION(#106,#12894);
#168=CONTEXT_DEPENDENT_SHAPE_REPRESENTATION(#107,#12895);
#169=CONTEXT_DEPENDENT_SHAPE_REPRESENTATION(#108,#12896);
#170=CONTEXT_DEPENDENT_SHAPE_REPRESENTATION(#109,#12897);
#171=CONTEXT_DEPENDENT_SHAPE_REPRESENTATION(#110,#12898);
#172=CONTEXT_DEPENDENT_SHAPE_REPRESENTATION(#111,#12899);
#173=CONTEXT_DEPENDENT_SHAPE_REPRESENTATION(#112,#12900);
#174=CONTEXT_DEPENDENT_SHAPE_REPRESENTATION(#113,#12901);
#175=CONTEXT_DEPENDENT_SHAPE_REPRESENTATION(#114,#12902);
#176=CONTEXT_DEPENDENT_SHAPE_REPRESENTATION(#115,#12903);
#177=CONTEXT_DEPENDENT_SHAPE_REPRESENTATION(#116,#12904);
#178=CONTEXT_DEPENDENT_SHAPE_REPRESENTATION(#117,#12905);
#179=CONTEXT_DEPENDENT_SHAPE_REPRESENTATION(#118,#12906);
#180=CONTEXT_DEPENDENT_SHAPE_REPRESENTATION(#119,#12907);
#181=CONTEXT_DEPENDENT_SHAPE_REPRESENTATION(#120,#12910);
#182=CONTEXT_DEPENDENT_SHAPE_REPRESENTATION(#121,#12911);
#183=CONTEXT_DEPENDENT_SHAPE_REPRESENTATION(#122,#12912);
#184=CONTEXT_DEPENDENT_SHAPE_REPRESENTATION(#123,#12913);
#185=CONTEXT_DEPENDENT_SHAPE_REPRESENTATION(#124,#12914);
#186=CONTEXT_DEPENDENT_SHAPE_REPRESENTATION(#125,#12915);
#187=CONTEXT_DEPENDENT_SHAPE_REPRESENTATION(#126,#12916);
#188=CONTEXT_DEPENDENT_SHAPE_REPRESENTATION(#127,#12917);
#189=CONTEXT_DEPENDENT_SHAPE_REPRESENTATION(#128,#12918);
#190=CONTEXT_DEPENDENT_SHAPE_REPRESENTATION(#129,#12919);
#191=CONTEXT_DEPENDENT_SHAPE_REPRESENTATION(#130,#12920);
#192=CONTEXT_DEPENDENT_SHAPE_REPRESENTATION(#131,#12921);
#193=CONTEXT_DEPENDENT_SHAPE_REPRESENTATION(#132,#12922);
#194=NEXT_ASSEMBLY_USAGE_OCCURRENCE('Inner ring:1','Inner ring:1',
'Inner ring:1',#12984,#12985,'Inner ring:1');
#195=NEXT_ASSEMBLY_USAGE_OCCURRENCE('Outer ring:1','Outer ring:1',
'Outer ring:1',#12984,#12986,'Outer ring:1');
#196=NEXT_ASSEMBLY_USAGE_OCCURRENCE('Balls:1','Balls:1','Balls:1',#12984,
#12987,'Balls:1');
#197=NEXT_ASSEMBLY_USAGE_OCCURRENCE('Cage:1','Cage:1','Cage:1',#12984,#12988,
'Cage:1');
#198=NEXT_ASSEMBLY_USAGE_OCCURRENCE('Seals 2RS:1','Seals 2RS:1',
'Seals 2RS:1',#12984,#12989,'Seals 2RS:1');
#199=NEXT_ASSEMBLY_USAGE_OCCURRENCE('Tensioner arm:1','Tensioner arm:1',
'Tensioner arm:1',#12977,#12978,'Tensioner arm:1');
#200=NEXT_ASSEMBLY_USAGE_OCCURRENCE('Bearing cap:1','Bearing cap:1',
'Bearing cap:1',#12977,#12979,'Bearing cap:1');
#201=NEXT_ASSEMBLY_USAGE_OCCURRENCE('Bearing cap (1):1',
'Bearing cap (1):1','Bearing cap (1):1',#12977,#12980,
'Bearing cap (1):1');
#202=NEXT_ASSEMBLY_USAGE_OCCURRENCE('Bearing cap (2):1',
'Bearing cap (2):1','Bearing cap (2):1',#12977,#12981,
'Bearing cap (2):1');
#203=NEXT_ASSEMBLY_USAGE_OCCURRENCE('Bearing cap (3):1',
'Bearing cap (3):1','Bearing cap (3):1',#12977,#12982,
'Bearing cap (3):1');
#204=NEXT_ASSEMBLY_USAGE_OCCURRENCE('Arm spring bracket:1',
'Arm spring bracket:1','Arm spring bracket:1',#12977,#12983,
'Arm spring bracket:1');
#205=NEXT_ASSEMBLY_USAGE_OCCURRENCE(
'Sealed Ball Bearing - 10 x 30 x 9 mm:2',
'Sealed Ball Bearing - 10 x 30 x 9 mm:2',
'Sealed Ball Bearing - 10 x 30 x 9 mm:2',#12977,#12984,
'Sealed Ball Bearing - 10 x 30 x 9 mm:2');
#206=NEXT_ASSEMBLY_USAGE_OCCURRENCE('M4x7 cap screw:2',
'M4x7 cap screw:2','M4x7 cap screw:2',#12977,#12990,'M4x7 cap screw:2');
#207=NEXT_ASSEMBLY_USAGE_OCCURRENCE('M4x7 cap screw:3',
'M4x7 cap screw:3','M4x7 cap screw:3',#12977,#12990,'M4x7 cap screw:3');
#208=NEXT_ASSEMBLY_USAGE_OCCURRENCE('M4x7 cap screw:4',
'M4x7 cap screw:4','M4x7 cap screw:4',#12977,#12990,'M4x7 cap screw:4');
#209=NEXT_ASSEMBLY_USAGE_OCCURRENCE('M4x7 cap screw:5',
'M4x7 cap screw:5','M4x7 cap screw:5',#12977,#12990,'M4x7 cap screw:5');
#210=NEXT_ASSEMBLY_USAGE_OCCURRENCE('M4x7 cap screw:6',
'M4x7 cap screw:6','M4x7 cap screw:6',#12977,#12990,'M4x7 cap screw:6');
#211=NEXT_ASSEMBLY_USAGE_OCCURRENCE('M4x7 cap screw:7',
'M4x7 cap screw:7','M4x7 cap screw:7',#12977,#12990,'M4x7 cap screw:7');
#212=NEXT_ASSEMBLY_USAGE_OCCURRENCE('M4x7 cap screw:8',
'M4x7 cap screw:8','M4x7 cap screw:8',#12977,#12990,'M4x7 cap screw:8');
#213=NEXT_ASSEMBLY_USAGE_OCCURRENCE('M4x7 cap screw:9',
'M4x7 cap screw:9','M4x7 cap screw:9',#12977,#12990,'M4x7 cap screw:9');
#214=NEXT_ASSEMBLY_USAGE_OCCURRENCE(
'Sealed Ball Bearing - 10 x 30 x 9 mm:3',
'Sealed Ball Bearing - 10 x 30 x 9 mm:3',
'Sealed Ball Bearing - 10 x 30 x 9 mm:3',#12977,#12984,
'Sealed Ball Bearing - 10 x 30 x 9 mm:3');
#215=NEXT_ASSEMBLY_USAGE_OCCURRENCE('M4x7 cap screw:10',
'M4x7 cap screw:10','M4x7 cap screw:10',#12977,#12990,
'M4x7 cap screw:10');
#216=NEXT_ASSEMBLY_USAGE_OCCURRENCE('M4x7 cap screw:11',
'M4x7 cap screw:11','M4x7 cap screw:11',#12977,#12990,
'M4x7 cap screw:11');
#217=NEXT_ASSEMBLY_USAGE_OCCURRENCE('M4x7 cap screw:12',
'M4x7 cap screw:12','M4x7 cap screw:12',#12977,#12990,
'M4x7 cap screw:12');
#218=NEXT_ASSEMBLY_USAGE_OCCURRENCE('M4x7 cap screw:13',
'M4x7 cap screw:13','M4x7 cap screw:13',#12977,#12990,
'M4x7 cap screw:13');
#219=NEXT_ASSEMBLY_USAGE_OCCURRENCE('M4x7 cap screw:14',
'M4x7 cap screw:14','M4x7 cap screw:14',#12977,#12990,
'M4x7 cap screw:14');
#220=NEXT_ASSEMBLY_USAGE_OCCURRENCE('M4x7 cap screw:15',
'M4x7 cap screw:15','M4x7 cap screw:15',#12977,#12990,
'M4x7 cap screw:15');
#221=NEXT_ASSEMBLY_USAGE_OCCURRENCE('M4x7 cap screw:16',
'M4x7 cap screw:16','M4x7 cap screw:16',#12977,#12990,
'M4x7 cap screw:16');
#222=NEXT_ASSEMBLY_USAGE_OCCURRENCE('M4x7 cap screw:17',
'M4x7 cap screw:17','M4x7 cap screw:17',#12977,#12990,
'M4x7 cap screw:17');
#223=NEXT_ASSEMBLY_USAGE_OCCURRENCE('Base:1','Base:1','Base:1',#12964,#12965,
'Base:1');
#224=NEXT_ASSEMBLY_USAGE_OCCURRENCE('Foot:1','Foot:1','Foot:1',#12964,#12966,
'Foot:1');
#225=NEXT_ASSEMBLY_USAGE_OCCURRENCE('Foot (1):1','Foot (1):1',
'Foot (1):1',#12964,#12967,'Foot (1):1');
#226=NEXT_ASSEMBLY_USAGE_OCCURRENCE('Pivot pedestal and pin:1',
'Pivot pedestal and pin:1','Pivot pedestal and pin:1',#12964,#12968,
'Pivot pedestal and pin:1');
#227=NEXT_ASSEMBLY_USAGE_OCCURRENCE('Pivot collar:1','Pivot collar:1',
'Pivot collar:1',#12964,#12969,'Pivot collar:1');
#228=NEXT_ASSEMBLY_USAGE_OCCURRENCE('Fixed spring post:1',
'Fixed spring post:1','Fixed spring post:1',#12964,#12970,
'Fixed spring post:1');
#229=NEXT_ASSEMBLY_USAGE_OCCURRENCE('Installed torsion spring:1',
'Installed torsion spring:1','Installed torsion spring:1',#12964,#12971,
'Installed torsion spring:1');
#230=NEXT_ASSEMBLY_USAGE_OCCURRENCE('Stop screw bracket:1',
'Stop screw bracket:1','Stop screw bracket:1',#12964,#12972,
'Stop screw bracket:1');
#231=NEXT_ASSEMBLY_USAGE_OCCURRENCE('Flat Washer - M5:2',
'Flat Washer - M5:2','Flat Washer - M5:2',#12964,#12973,
'Flat Washer - M5:2');
#232=NEXT_ASSEMBLY_USAGE_OCCURRENCE('Cap Screw - M5x20:2',
'Cap Screw - M5x20:2','Cap Screw - M5x20:2',#12964,#12974,
'Cap Screw - M5x20:2');
#233=NEXT_ASSEMBLY_USAGE_OCCURRENCE('Flat Washer - M5:3',
'Flat Washer - M5:3','Flat Washer - M5:3',#12964,#12973,
'Flat Washer - M5:3');
#234=NEXT_ASSEMBLY_USAGE_OCCURRENCE('Cap Screw - M5x20:3',
'Cap Screw - M5x20:3','Cap Screw - M5x20:3',#12964,#12974,
'Cap Screw - M5x20:3');
#235=NEXT_ASSEMBLY_USAGE_OCCURRENCE('Flat Washer - M5:4',
'Flat Washer - M5:4','Flat Washer - M5:4',#12964,#12973,
'Flat Washer - M5:4');
#236=NEXT_ASSEMBLY_USAGE_OCCURRENCE('Cap Screw - M5x20:4',
'Cap Screw - M5x20:4','Cap Screw - M5x20:4',#12964,#12974,
'Cap Screw - M5x20:4');
#237=NEXT_ASSEMBLY_USAGE_OCCURRENCE('M4x4 collar screw:2',
'M4x4 collar screw:2','M4x4 collar screw:2',#12964,#12999,
'M4x4 collar screw:2');
#238=NEXT_ASSEMBLY_USAGE_OCCURRENCE('Cap Screw - M4x16:2',
'Cap Screw - M4x16:2','Cap Screw - M4x16:2',#12964,#12976,
'Cap Screw - M4x16:2');
#239=NEXT_ASSEMBLY_USAGE_OCCURRENCE('Cap Screw - M5x20:5',
'Cap Screw - M5x20:5','Cap Screw - M5x20:5',#12964,#12974,
'Cap Screw - M5x20:5');
#240=NEXT_ASSEMBLY_USAGE_OCCURRENCE('Hex Nut - M5:2','Hex Nut - M5:2',
'Hex Nut - M5:2',#12964,#12975,'Hex Nut - M5:2');
#241=NEXT_ASSEMBLY_USAGE_OCCURRENCE('Cap Screw - M4x16:3',
'Cap Screw - M4x16:3','Cap Screw - M4x16:3',#12964,#12976,
'Cap Screw - M4x16:3');
#242=NEXT_ASSEMBLY_USAGE_OCCURRENCE('Stepped idler axle:1',
'Stepped idler axle:1','Stepped idler axle:1',#12991,#12992,
'Stepped idler axle:1');
#243=NEXT_ASSEMBLY_USAGE_OCCURRENCE('Idler collar:1','Idler collar:1',
'Idler collar:1',#12991,#12993,'Idler collar:1');
#244=NEXT_ASSEMBLY_USAGE_OCCURRENCE('Lower pulley spacer:1',
'Lower pulley spacer:1','Lower pulley spacer:1',#12991,#12994,
'Lower pulley spacer:1');
#245=NEXT_ASSEMBLY_USAGE_OCCURRENCE('Upper pulley spacer:1',
'Upper pulley spacer:1','Upper pulley spacer:1',#12991,#12995,
'Upper pulley spacer:1');
#246=NEXT_ASSEMBLY_USAGE_OCCURRENCE('M3 pulley set screw:1',
'M3 pulley set screw:1','M3 pulley set screw:1',#12991,#12996,
'M3 pulley set screw:1');
#247=NEXT_ASSEMBLY_USAGE_OCCURRENCE('M3 pulley set screw (1):1',
'M3 pulley set screw (1):1','M3 pulley set screw (1):1',#12991,#12997,
'M3 pulley set screw (1):1');
#248=NEXT_ASSEMBLY_USAGE_OCCURRENCE('Axle keeper:1','Axle keeper:1',
'Axle keeper:1',#12991,#12998,'Axle keeper:1');
#249=NEXT_ASSEMBLY_USAGE_OCCURRENCE('M4x4 collar screw:3',
'M4x4 collar screw:3','M4x4 collar screw:3',#12991,#12999,
'M4x4 collar screw:3');
#250=NEXT_ASSEMBLY_USAGE_OCCURRENCE(
'Timing Pulley - 2 mm Pitch, 20 Teeth, 8 mm Bore:2',
'Timing Pulley - 2 mm Pitch, 20 Teeth, 8 mm Bore:2',
'Timing Pulley - 2 mm Pitch, 20 Teeth, 8 mm Bore:2',#12991,#13000,
'Timing Pulley - 2 mm Pitch, 20 Teeth, 8 mm Bore:2');
#251=NEXT_ASSEMBLY_USAGE_OCCURRENCE('M4x10 Cap Screw:2',
'M4x10 Cap Screw:2','M4x10 Cap Screw:2',#12991,#13001,
'M4x10 Cap Screw:2');
#252=NEXT_ASSEMBLY_USAGE_OCCURRENCE(
'Pivot frame and installed torsion spring:1',
'Pivot frame and installed torsion spring:1',
'Pivot frame and installed torsion spring:1',#12963,#12964,
'Pivot frame and installed torsion spring:1');
#253=NEXT_ASSEMBLY_USAGE_OCCURRENCE('Pivoting arm:1','Pivoting arm:1',
'Pivoting arm:1',#12963,#12977,'Pivoting arm:1');
#254=NEXT_ASSEMBLY_USAGE_OCCURRENCE('Bearing-mounted idler:1',
'Bearing-mounted idler:1','Bearing-mounted idler:1',#12963,#12991,
'Bearing-mounted idler:1');
#255=SPHERICAL_SURFACE('',#7008,0.23815);
#256=SPHERICAL_SURFACE('',#7010,0.23815);
#257=SPHERICAL_SURFACE('',#7012,0.23815);
#258=SPHERICAL_SURFACE('',#7014,0.23815);
#259=SPHERICAL_SURFACE('',#7016,0.23815);
#260=SPHERICAL_SURFACE('',#7018,0.23815);
#261=SPHERICAL_SURFACE('',#7020,0.23815);
#262=SPHERICAL_SURFACE('',#7022,0.23815);
#263=SPHERICAL_SURFACE('',#7025,0.247676);
#264=SPHERICAL_SURFACE('',#7041,0.247676);
#265=SPHERICAL_SURFACE('',#7046,0.247676);
#266=SPHERICAL_SURFACE('',#7051,0.247676);
#267=SPHERICAL_SURFACE('',#7056,0.247676);
#268=SPHERICAL_SURFACE('',#7061,0.247676);
#269=SPHERICAL_SURFACE('',#7066,0.247676);
#270=SPHERICAL_SURFACE('',#7074,0.247676);
#271=TOROIDAL_SURFACE('',#6968,1.,0.247676);
#272=TOROIDAL_SURFACE('',#6988,1.,0.247676);
#273=(
BOUNDED_CURVE()
B_SPLINE_CURVE(2,(#10544,#10545,#10546),.UNSPECIFIED.,.F.,.F.)
B_SPLINE_CURVE_WITH_KNOTS((3,3),(0.140651836354967,0.670383167684795),
 .UNSPECIFIED.)
CURVE()
GEOMETRIC_REPRESENTATION_ITEM()
RATIONAL_B_SPLINE_CURVE((1.11602540378444,1.28867513459481,1.11602540378444))
REPRESENTATION_ITEM('')
);
#274=(
BOUNDED_CURVE()
B_SPLINE_CURVE(2,(#10548,#10549,#10550),.UNSPECIFIED.,.F.,.F.)
B_SPLINE_CURVE_WITH_KNOTS((3,3),(0.140651836354967,0.670383167684795),
 .UNSPECIFIED.)
CURVE()
GEOMETRIC_REPRESENTATION_ITEM()
RATIONAL_B_SPLINE_CURVE((1.11602540378444,1.28867513459481,1.11602540378444))
REPRESENTATION_ITEM('')
);
#275=(
BOUNDED_CURVE()
B_SPLINE_CURVE(2,(#10555,#10556,#10557),.UNSPECIFIED.,.F.,.F.)
B_SPLINE_CURVE_WITH_KNOTS((3,3),(0.140651836354967,0.670383167684795),
 .UNSPECIFIED.)
CURVE()
GEOMETRIC_REPRESENTATION_ITEM()
RATIONAL_B_SPLINE_CURVE((1.11602540378444,1.28867513459481,1.11602540378444))
REPRESENTATION_ITEM('')
);
#276=(
BOUNDED_CURVE()
B_SPLINE_CURVE(2,(#10559,#10560,#10561),.UNSPECIFIED.,.F.,.F.)
B_SPLINE_CURVE_WITH_KNOTS((3,3),(0.140651836354967,0.670383167684795),
 .UNSPECIFIED.)
CURVE()
GEOMETRIC_REPRESENTATION_ITEM()
RATIONAL_B_SPLINE_CURVE((1.11602540378444,1.28867513459481,1.11602540378444))
REPRESENTATION_ITEM('')
);
#277=(
BOUNDED_CURVE()
B_SPLINE_CURVE(2,(#10563,#10564,#10565),.UNSPECIFIED.,.F.,.F.)
B_SPLINE_CURVE_WITH_KNOTS((3,3),(0.140651836354967,0.670383167684795),
 .UNSPECIFIED.)
CURVE()
GEOMETRIC_REPRESENTATION_ITEM()
RATIONAL_B_SPLINE_CURVE((1.11602540378444,1.28867513459481,1.11602540378444))
REPRESENTATION_ITEM('')
);
#278=(
BOUNDED_CURVE()
B_SPLINE_CURVE(2,(#10566,#10567,#10568),.UNSPECIFIED.,.F.,.F.)
B_SPLINE_CURVE_WITH_KNOTS((3,3),(0.140651836354967,0.670383167684795),
 .UNSPECIFIED.)
CURVE()
GEOMETRIC_REPRESENTATION_ITEM()
RATIONAL_B_SPLINE_CURVE((1.11602540378444,1.28867513459481,1.11602540378444))
REPRESENTATION_ITEM('')
);
#279=(
BOUNDED_CURVE()
B_SPLINE_CURVE(2,(#10575,#10576,#10577),.UNSPECIFIED.,.F.,.F.)
B_SPLINE_CURVE_WITH_KNOTS((3,3),(0.140651836354967,0.670383167684795),
 .UNSPECIFIED.)
CURVE()
GEOMETRIC_REPRESENTATION_ITEM()
RATIONAL_B_SPLINE_CURVE((1.11602540378444,1.28867513459481,1.11602540378444))
REPRESENTATION_ITEM('')
);
#280=(
BOUNDED_CURVE()
B_SPLINE_CURVE(2,(#10579,#10580,#10581),.UNSPECIFIED.,.F.,.F.)
B_SPLINE_CURVE_WITH_KNOTS((3,3),(0.140651836354967,0.670383167684796),
 .UNSPECIFIED.)
CURVE()
GEOMETRIC_REPRESENTATION_ITEM()
RATIONAL_B_SPLINE_CURVE((1.11602540378444,1.28867513459481,1.11602540378444))
REPRESENTATION_ITEM('')
);
#281=(
BOUNDED_CURVE()
B_SPLINE_CURVE(2,(#10583,#10584,#10585),.UNSPECIFIED.,.F.,.F.)
B_SPLINE_CURVE_WITH_KNOTS((3,3),(0.140651836354967,0.670383167684795),
 .UNSPECIFIED.)
CURVE()
GEOMETRIC_REPRESENTATION_ITEM()
RATIONAL_B_SPLINE_CURVE((1.11602540378444,1.28867513459481,1.11602540378444))
REPRESENTATION_ITEM('')
);
#282=(
BOUNDED_CURVE()
B_SPLINE_CURVE(2,(#10587,#10588,#10589),.UNSPECIFIED.,.F.,.F.)
B_SPLINE_CURVE_WITH_KNOTS((3,3),(0.140651836354967,0.670383167684795),
 .UNSPECIFIED.)
CURVE()
GEOMETRIC_REPRESENTATION_ITEM()
RATIONAL_B_SPLINE_CURVE((1.11602540378444,1.28867513459482,1.11602540378444))
REPRESENTATION_ITEM('')
);
#283=(
BOUNDED_CURVE()
B_SPLINE_CURVE(2,(#10591,#10592,#10593),.UNSPECIFIED.,.F.,.F.)
B_SPLINE_CURVE_WITH_KNOTS((3,3),(0.140651836354967,0.670383167684795),
 .UNSPECIFIED.)
CURVE()
GEOMETRIC_REPRESENTATION_ITEM()
RATIONAL_B_SPLINE_CURVE((1.11602540378444,1.28867513459481,1.11602540378444))
REPRESENTATION_ITEM('')
);
#284=(
BOUNDED_CURVE()
B_SPLINE_CURVE(2,(#10594,#10595,#10596),.UNSPECIFIED.,.F.,.F.)
B_SPLINE_CURVE_WITH_KNOTS((3,3),(0.140651836354967,0.670383167684795),
 .UNSPECIFIED.)
CURVE()
GEOMETRIC_REPRESENTATION_ITEM()
RATIONAL_B_SPLINE_CURVE((1.11602540378444,1.28867513459481,1.11602540378444))
REPRESENTATION_ITEM('')
);
#285=ORIENTED_CLOSED_SHELL('',*,#6191,.F.);
#286=ORIENTED_CLOSED_SHELL('',*,#6194,.F.);
#287=ORIENTED_CLOSED_SHELL('',*,#6215,.F.);
#288=ORIENTED_CLOSED_SHELL('',*,#6225,.F.);
#289=BREP_WITH_VOIDS('Body1',#6190,(#285));
#290=BREP_WITH_VOIDS('Body1',#6193,(#286));
#291=BREP_WITH_VOIDS('Body1',#6214,(#287));
#292=BREP_WITH_VOIDS('Body1',#6226,(#288));
#293=CONICAL_SURFACE('',#6730,0.275,0.785398163397449);
#294=CONICAL_SURFACE('',#6743,0.4,0.785398163397448);
#295=CONICAL_SURFACE('',#6747,0.41,0.785398163397448);
#296=CONICAL_SURFACE('',#6751,0.26,0.463647609000806);
#297=CONICAL_SURFACE('',#6755,0.225,0.785398163397448);
#298=CONICAL_SURFACE('',#6767,0.47094010767585,1.0471975511966);
#299=CONICAL_SURFACE('',#6769,0.47094010767585,1.0471975511966);
#300=CONICAL_SURFACE('',#6785,0.325,0.785398163397448);
#301=CONICAL_SURFACE('',#6789,0.335,0.785398163397448);
#302=CONICAL_SURFACE('',#6793,0.21,0.463647609000806);
#303=CONICAL_SURFACE('',#6797,0.18,0.785398163397448);
#304=CONICAL_SURFACE('',#6979,0.53,0.785398163397448);
#305=CONICAL_SURFACE('',#6986,0.53,0.785398163397448);
#306=CONICAL_SURFACE('',#6999,1.47,0.785398163397449);
#307=CONICAL_SURFACE('',#7003,1.47,0.785398163397449);
#308=CONICAL_SURFACE('',#7105,0.325,0.785398163397448);
#309=CONICAL_SURFACE('',#7109,0.335,0.785398163397448);
#310=CONICAL_SURFACE('',#7113,0.21,0.463647609000806);
#311=CONICAL_SURFACE('',#7232,0.185,0.785398163397449);
#312=CONICAL_SURFACE('',#7409,0.325,0.785398163397448);
#313=CONICAL_SURFACE('',#7413,0.335,0.785398163397448);
#314=CONICAL_SURFACE('',#7417,0.21,0.463647609000806);
#315=B_SPLINE_SURFACE_WITH_KNOTS('',3,3,((#9880,#9881,#9882,#9883,#9884,
#9885,#9886,#9887,#9888,#9889,#9890,#9891,#9892,#9893,#9894,#9895,#9896,
#9897,#9898,#9899,#9900,#9901,#9902,#9903,#9904,#9905,#9906,#9907,#9908,
#9909,#9910,#9911,#9912,#9913,#9914,#9915,#9916,#9917,#9918,#9919,#9920),
(#9921,#9922,#9923,#9924,#9925,#9926,#9927,#9928,#9929,#9930,#9931,#9932,
#9933,#9934,#9935,#9936,#9937,#9938,#9939,#9940,#9941,#9942,#9943,#9944,
#9945,#9946,#9947,#9948,#9949,#9950,#9951,#9952,#9953,#9954,#9955,#9956,
#9957,#9958,#9959,#9960,#9961),(#9962,#9963,#9964,#9965,#9966,#9967,#9968,
#9969,#9970,#9971,#9972,#9973,#9974,#9975,#9976,#9977,#9978,#9979,#9980,
#9981,#9982,#9983,#9984,#9985,#9986,#9987,#9988,#9989,#9990,#9991,#9992,
#9993,#9994,#9995,#9996,#9997,#9998,#9999,#10000,#10001,#10002),(#10003,
#10004,#10005,#10006,#10007,#10008,#10009,#10010,#10011,#10012,#10013,#10014,
#10015,#10016,#10017,#10018,#10019,#10020,#10021,#10022,#10023,#10024,#10025,
#10026,#10027,#10028,#10029,#10030,#10031,#10032,#10033,#10034,#10035,#10036,
#10037,#10038,#10039,#10040,#10041,#10042,#10043),(#10044,#10045,#10046,
#10047,#10048,#10049,#10050,#10051,#10052,#10053,#10054,#10055,#10056,#10057,
#10058,#10059,#10060,#10061,#10062,#10063,#10064,#10065,#10066,#10067,#10068,
#10069,#10070,#10071,#10072,#10073,#10074,#10075,#10076,#10077,#10078,#10079,
#10080,#10081,#10082,#10083,#10084),(#10085,#10086,#10087,#10088,#10089,
#10090,#10091,#10092,#10093,#10094,#10095,#10096,#10097,#10098,#10099,#10100,
#10101,#10102,#10103,#10104,#10105,#10106,#10107,#10108,#10109,#10110,#10111,
#10112,#10113,#10114,#10115,#10116,#10117,#10118,#10119,#10120,#10121,#10122,
#10123,#10124,#10125),(#10126,#10127,#10128,#10129,#10130,#10131,#10132,
#10133,#10134,#10135,#10136,#10137,#10138,#10139,#10140,#10141,#10142,#10143,
#10144,#10145,#10146,#10147,#10148,#10149,#10150,#10151,#10152,#10153,#10154,
#10155,#10156,#10157,#10158,#10159,#10160,#10161,#10162,#10163,#10164,#10165,
#10166),(#10167,#10168,#10169,#10170,#10171,#10172,#10173,#10174,#10175,
#10176,#10177,#10178,#10179,#10180,#10181,#10182,#10183,#10184,#10185,#10186,
#10187,#10188,#10189,#10190,#10191,#10192,#10193,#10194,#10195,#10196,#10197,
#10198,#10199,#10200,#10201,#10202,#10203,#10204,#10205,#10206,#10207),
(#10208,#10209,#10210,#10211,#10212,#10213,#10214,#10215,#10216,#10217,
#10218,#10219,#10220,#10221,#10222,#10223,#10224,#10225,#10226,#10227,#10228,
#10229,#10230,#10231,#10232,#10233,#10234,#10235,#10236,#10237,#10238,#10239,
#10240,#10241,#10242,#10243,#10244,#10245,#10246,#10247,#10248),(#10249,
#10250,#10251,#10252,#10253,#10254,#10255,#10256,#10257,#10258,#10259,#10260,
#10261,#10262,#10263,#10264,#10265,#10266,#10267,#10268,#10269,#10270,#10271,
#10272,#10273,#10274,#10275,#10276,#10277,#10278,#10279,#10280,#10281,#10282,
#10283,#10284,#10285,#10286,#10287,#10288,#10289)),.UNSPECIFIED.,.T.,.F.,
 .F.,(4,1,1,1,1,1,1,4),(4,1,1,1,1,1,1,1,1,1,1,1,1,1,1,1,1,1,1,1,1,1,1,1,
1,1,1,1,1,1,1,1,1,1,1,1,1,1,4),(-3.14159265358988,-2.24399475256421,-1.34639685153853,
-0.448798950512863,0.448798950512809,1.34639685153848,2.24399475256415,
3.14159265358982),(0.,0.0357142857142857,0.0714285714285714,0.107142857142857,
0.125,0.133928571428571,0.142857142857143,0.174603174603175,0.19047619047619,
0.214285714285714,0.238095238095238,0.261904761904762,0.273809523809524,
0.285714285714286,0.30952380952381,0.333333333333333,0.357142857142857,
0.380952380952381,0.412698412698413,0.428571428571429,0.452380952380952,
0.476190476190476,0.5,0.535714285714286,0.571428571428571,0.607142857142857,
0.642857142857143,0.678571428571428,0.714285714285714,0.738095238095238,
0.761904761904762,0.785714285714286,0.809523809523809,0.833333333333333,
0.857142857142857,0.892857142857143,0.928571428571429,0.964285714285714,
1.),.UNSPECIFIED.);
#316=ELLIPSE('',#6695,0.0848528137423855,0.0599999999999996);
#317=B_SPLINE_CURVE_WITH_KNOTS('',3,(#9613,#9614,#9615,#9616,#9617,#9618,
#9619,#9620,#9621,#9622,#9623,#9624,#9625,#9626),.UNSPECIFIED.,.F.,.F.,
(4,2,2,2,2,2,4),(0.618551524396292,0.626563103102765,0.689203386094988,
0.751843669087211,0.814483952079434,0.877124235071657,0.88513581377813),
 .UNSPECIFIED.);
#318=B_SPLINE_CURVE_WITH_KNOTS('',3,(#9630,#9631,#9632,#9633,#9634,#9635,
#9636,#9637),.UNSPECIFIED.,.F.,.F.,(4,2,2,4),(0.250614556362404,0.313254839354627,
0.37589512234685,0.383906701053323),.UNSPECIFIED.);
#319=B_SPLINE_CURVE_WITH_KNOTS('',3,(#9641,#9642,#9643,#9644,#9645,#9646,
#9647,#9648,#9649,#9650,#9651,#9652,#9653,#9654,#9655,#9656,#9657,#9658,
#9659,#9660,#9661,#9662,#9663,#9664,#9665,#9666),.UNSPECIFIED.,.F.,.F.,
(4,2,2,2,2,2,2,2,2,2,2,2,4),(0.,0.0623062782223143,0.124612556444629,0.186916384615149,
0.249220212785669,0.31152404095619,0.37382786912671,0.436134147349024,0.498440425571339,
0.560746703793653,0.623052982015967,0.685356810186488,0.747660638357008),
 .UNSPECIFIED.);
#320=B_SPLINE_CURVE_WITH_KNOTS('',3,(#9667,#9668,#9669,#9670,#9671,#9672,
#9673,#9674,#9675,#9676),.UNSPECIFIED.,.F.,.F.,(4,2,2,2,4),(0.747660638357008,
0.809964466527528,0.872268294698049,0.934574572920363,0.996880851142677),
 .UNSPECIFIED.);
#321=B_SPLINE_CURVE_WITH_KNOTS('',3,(#9677,#9678,#9679,#9680,#9681,#9682,
#9683,#9684),.UNSPECIFIED.,.F.,.F.,(4,2,2,4),(0.117322411671484,0.125333990377958,
0.187974273370181,0.250614556362404),.UNSPECIFIED.);
#322=B_SPLINE_CURVE_WITH_KNOTS('',3,(#9711,#9712,#9713,#9714,#9715,#9716,
#9717,#9718,#9719,#9720,#9721,#9722,#9723,#9724,#9725,#9726,#9727,#9728,
#9729,#9730,#9731,#9732,#9733,#9734,#9735,#9736,#9737,#9738,#9739,#9740,
#9741,#9742,#9743,#9744),.UNSPECIFIED.,.T.,.F.,(4,2,2,2,2,2,2,2,2,2,2,2,
2,2,2,2,4),(0.,0.0264055269244546,0.0528110538489091,0.0792162323581904,
0.105621410867472,0.132026589376753,0.158431767886034,0.184837294810489,
0.211242821734944,0.237648348659398,0.264053875583852,0.290459054093133,
0.316864232602415,0.343269411111696,0.369674589620977,0.396080116545432,
0.422485643469887),.UNSPECIFIED.);
#323=B_SPLINE_CURVE_WITH_KNOTS('',3,(#9747,#9748,#9749,#9750,#9751,#9752,
#9753,#9754,#9755,#9756,#9757,#9758,#9759,#9760,#9761,#9762,#9763,#9764,
#9765,#9766,#9767,#9768,#9769,#9770,#9771,#9772,#9773,#9774,#9775,#9776,
#9777,#9778,#9779,#9780),.UNSPECIFIED.,.T.,.F.,(4,2,2,2,2,2,2,2,2,2,2,2,
2,2,2,2,4),(0.,0.0264055269244546,0.0528110538489091,0.0792162323581904,
0.105621410867472,0.132026589376753,0.158431767886035,0.184837294810489,
0.211242821734943,0.237648348659398,0.264053875583852,0.290459054093133,
0.316864232602415,0.343269411111696,0.369674589620977,0.396080116545432,
0.422485643469887),.UNSPECIFIED.);
#324=B_SPLINE_CURVE_WITH_KNOTS('',3,(#9810,#9811,#9812,#9813,#9814,#9815,
#9816),.UNSPECIFIED.,.F.,.F.,(4,3,4),(-0.00330054689312876,0.,0.00113632995669113),
 .UNSPECIFIED.);
#325=B_SPLINE_CURVE_WITH_KNOTS('',3,(#9817,#9818,#9819,#9820,#9821,#9822,
#9823,#9824,#9825,#9826,#9827,#9828,#9829,#9830,#9831,#9832,#9833,#9834,
#9835,#9836,#9837,#9838,#9839,#9840,#9841,#9842,#9843,#9844,#9845,#9846,
#9847,#9848,#9849,#9850,#9851,#9852,#9853,#9854,#9855,#9856,#9857,#9858,
#9859,#9860,#9861,#9862,#9863,#9864,#9865,#9866,#9867,#9868,#9869,#9870,
#9871,#9872,#9873,#9874),.UNSPECIFIED.,.F.,.F.,(4,3,3,3,3,3,3,3,3,3,3,3,
3,3,3,3,3,3,3,4),(-0.187914936482157,-0.186780639062755,-0.170605853942537,
-0.165437814146277,-0.164113083876462,-0.147906084064185,-0.140662734614346,
-0.124376338567638,-0.117231977811975,-0.111403976662175,-0.095176489596115,
-0.0938100295088016,-0.0774833765802454,-0.070381765801811,-0.0573630234982956,
-0.046936415200375,-0.0306169940923779,-0.0234729466450609,-0.00725345698800663,
-0.00330054689312876),.UNSPECIFIED.);
#326=B_SPLINE_CURVE_WITH_KNOTS('',3,(#10292,#10293,#10294,#10295,#10296,
#10297,#10298,#10299,#10300,#10301,#10302,#10303,#10304,#10305,#10306,#10307,
#10308,#10309,#10310,#10311,#10312,#10313,#10314,#10315,#10316,#10317,#10318,
#10319,#10320,#10321,#10322,#10323,#10324,#10325,#10326,#10327,#10328,#10329,
#10330,#10331,#10332,#10333,#10334,#10335,#10336,#10337,#10338,#10339,#10340,
#10341,#10342,#10343,#10344,#10345,#10346,#10347,#10348,#10349,#10350,#10351,
#10352),.UNSPECIFIED.,.F.,.F.,(4,3,3,3,3,3,3,3,3,3,3,3,3,3,3,3,3,3,3,3,
4),(-0.187914936422243,-0.186780639028976,-0.174403055129874,-0.164113083856377,
-0.147782436669538,-0.140662734596942,-0.124476652868443,-0.120351214576537,
-0.117231977796532,-0.101004644530292,-0.0938100294949805,-0.0775453096070019,
-0.0703817657897228,-0.0663337540103528,-0.0501165597360029,-0.0469364151905663,
-0.0306116886006247,-0.0234729466383474,-0.0122741858231731,0.,0.00113632996403919),
 .UNSPECIFIED.);
#327=B_SPLINE_CURVE_WITH_KNOTS('',3,(#10356,#10357,#10358,#10359,#10360,
#10361,#10362,#10363,#10364,#10365,#10366,#10367,#10368,#10369,#10370,#10371,
#10372,#10373,#10374,#10375,#10376,#10377,#10378,#10379,#10380,#10381,#10382,
#10383,#10384,#10385,#10386,#10387,#10388,#10389,#10390,#10391,#10392,#10393,
#10394,#10395,#10396),.UNSPECIFIED.,.F.,.F.,(4,1,1,1,1,1,1,1,1,1,1,1,1,
1,1,1,1,1,1,1,1,1,1,1,1,1,1,1,1,1,1,1,1,1,1,1,1,1,4),(0.,0.0357142857142857,
0.0714285714285714,0.107142857142857,0.125,0.133928571428571,0.142857142857143,
0.174603174603175,0.19047619047619,0.214285714285714,0.238095238095238,
0.261904761904762,0.273809523809524,0.285714285714286,0.30952380952381,
0.333333333333333,0.357142857142857,0.380952380952381,0.412698412698413,
0.428571428571429,0.452380952380952,0.476190476190476,0.5,0.535714285714286,
0.571428571428571,0.607142857142857,0.642857142857143,0.678571428571428,
0.714285714285714,0.738095238095238,0.761904761904762,0.785714285714286,
0.809523809523809,0.833333333333333,0.857142857142857,0.892857142857143,
0.928571428571429,0.964285714285714,0.999978445633173),.UNSPECIFIED.);
#328=B_SPLINE_CURVE_WITH_KNOTS('',3,(#10397,#10398,#10399,#10400),
 .UNSPECIFIED.,.F.,.F.,(4,4),(0.999978445544819,0.999989048312129),
 .UNSPECIFIED.);
#329=B_SPLINE_CURVE_WITH_KNOTS('',3,(#10963,#10964,#10965,#10966,#10967,
#10968,#10969,#10970,#10971,#10972),.UNSPECIFIED.,.F.,.F.,(4,2,2,2,4),(0.,
0.0264055269244542,0.0528110538489084,0.0792162323581899,0.105621410867471),
 .UNSPECIFIED.);
#330=B_SPLINE_CURVE_WITH_KNOTS('',3,(#10974,#10975,#10976,#10977,#10978,
#10979,#10980,#10981,#10982,#10983),.UNSPECIFIED.,.F.,.F.,(4,2,2,2,4),(0.316864232602415,
0.343269411111696,0.369674589620978,0.396080116545432,0.422485643469886),
 .UNSPECIFIED.);
#331=B_SPLINE_CURVE_WITH_KNOTS('',3,(#10984,#10985,#10986,#10987,#10988,
#10989,#10990,#10991,#10992,#10993,#10994,#10995,#10996,#10997,#10998,#10999,
#11000,#11001),.UNSPECIFIED.,.F.,.F.,(4,2,2,2,2,2,2,2,4),(0.105621410867471,
0.132026589376753,0.158431767886035,0.184837294810489,0.211242821734943,
0.237648348659397,0.264053875583851,0.290459054093133,0.316864232602415),
 .UNSPECIFIED.);
#332=B_SPLINE_CURVE_WITH_KNOTS('',3,(#11005,#11006,#11007,#11008,#11009,
#11010,#11011,#11012,#11013,#11014,#11015,#11016,#11017,#11018,#11019,#11020,
#11021,#11022,#11023,#11024,#11025,#11026,#11027,#11028,#11029,#11030),
 .UNSPECIFIED.,.F.,.F.,(4,2,2,2,2,2,2,2,2,2,2,2,4),(0.,0.0264055269244542,
0.0528110538489084,0.0792162323581899,0.105621410867471,0.132026589376753,
0.158431767886035,0.184837294810489,0.211242821734943,0.237648348659397,
0.264053875583852,0.290459054093133,0.316864232602415),.UNSPECIFIED.);
#333=B_SPLINE_CURVE_WITH_KNOTS('',3,(#11031,#11032,#11033,#11034,#11035,
#11036,#11037,#11038,#11039,#11040),.UNSPECIFIED.,.F.,.F.,(4,2,2,2,4),(0.316864232602415,
0.343269411111696,0.369674589620978,0.396080116545432,0.422485643469886),
 .UNSPECIFIED.);
#334=B_SPLINE_CURVE_WITH_KNOTS('',3,(#11192,#11193,#11194,#11195,#11196,
#11197,#11198,#11199,#11200,#11201,#11202,#11203,#11204,#11205,#11206,#11207,
#11208,#11209,#11210,#11211,#11212,#11213),.UNSPECIFIED.,.F.,.F.,(4,2,2,
2,2,2,2,2,2,2,4),(0.0473477652366656,0.126350602536658,0.189525903804987,
0.252701205073317,0.313298422430275,0.373895639787233,0.434492857144191,
0.495090074501149,0.558265375769478,0.621440677037807,0.7004435143378),
 .UNSPECIFIED.);
#335=B_SPLINE_CURVE_WITH_KNOTS('',3,(#11217,#11218,#11219,#11220,#11221,
#11222,#11223,#11224,#11225,#11226,#11227,#11228,#11229,#11230,#11231,#11232,
#11233,#11234,#11235,#11236,#11237,#11238),.UNSPECIFIED.,.F.,.F.,(4,2,2,
2,2,2,2,2,2,2,4),(0.0464897534940957,0.0852567806515119,0.170513561303024,
0.246687263103517,0.308657850341199,0.370628437578881,0.432599024816563,
0.494569612054245,0.570743313854739,0.656000094506251,0.694767121663666),
 .UNSPECIFIED.);
#336=B_SPLINE_CURVE_WITH_KNOTS('',3,(#11244,#11245,#11246,#11247,#11248,
#11249,#11250,#11251,#11252,#11253,#11254,#11255,#11256,#11257,#11258,#11259,
#11260,#11261,#11262,#11263,#11264,#11265),.UNSPECIFIED.,.F.,.F.,(4,2,2,
2,2,2,2,2,2,2,4),(0.0464897534940957,0.0852567806515118,0.170513561303024,
0.246687263103517,0.308657850341199,0.370628437578881,0.432599024816563,
0.494569612054245,0.570743313854738,0.65600009450625,0.694767121663666),
 .UNSPECIFIED.);
#337=B_SPLINE_CURVE_WITH_KNOTS('',3,(#11269,#11270,#11271,#11272,#11273,
#11274,#11275,#11276,#11277,#11278,#11279,#11280,#11281,#11282,#11283,#11284,
#11285,#11286,#11287,#11288,#11289,#11290),.UNSPECIFIED.,.F.,.F.,(4,2,2,
2,2,2,2,2,2,2,4),(0.0464897534940957,0.0852567806515119,0.170513561303024,
0.246687263103517,0.308657850341199,0.370628437578881,0.432599024816563,
0.494569612054245,0.570743313854739,0.656000094506251,0.694767121663666),
 .UNSPECIFIED.);
#338=B_SPLINE_CURVE_WITH_KNOTS('',3,(#11294,#11295,#11296,#11297,#11298,
#11299,#11300,#11301,#11302,#11303,#11304,#11305),.UNSPECIFIED.,.F.,.F.,
(4,2,2,2,2,4),(0.0464897534940957,0.0852567806515119,0.170513561303024,
0.246687263103517,0.308657850341199,0.370628437578881),.UNSPECIFIED.);
#339=B_SPLINE_CURVE_WITH_KNOTS('',3,(#11310,#11311,#11312,#11313,#11314,
#11315,#11316,#11317,#11318,#11319,#11320,#11321),.UNSPECIFIED.,.F.,.F.,
(4,2,2,2,2,4),(0.370628437578881,0.432599024816563,0.494569612054245,0.570743313854738,
0.65600009450625,0.694767121663666),.UNSPECIFIED.);
#340=B_SPLINE_CURVE_WITH_KNOTS('',3,(#11325,#11326,#11327,#11328,#11329,
#11330,#11331,#11332,#11333,#11334,#11335,#11336,#11337,#11338,#11339,#11340,
#11341,#11342,#11343,#11344,#11345,#11346),.UNSPECIFIED.,.F.,.F.,(4,2,2,
2,2,2,2,2,2,2,4),(0.0464897534940957,0.0852567806515121,0.170513561303024,
0.246687263103518,0.308657850341199,0.370628437578881,0.432599024816563,
0.494569612054245,0.570743313854738,0.65600009450625,0.694767121663666),
 .UNSPECIFIED.);
#341=B_SPLINE_CURVE_WITH_KNOTS('',3,(#11350,#11351,#11352,#11353,#11354,
#11355,#11356,#11357,#11358,#11359,#11360,#11361,#11362,#11363,#11364,#11365,
#11366,#11367,#11368,#11369,#11370,#11371),.UNSPECIFIED.,.F.,.F.,(4,2,2,
2,2,2,2,2,2,2,4),(0.0464897534940957,0.0852567806515119,0.170513561303024,
0.246687263103517,0.308657850341199,0.370628437578881,0.432599024816563,
0.494569612054245,0.570743313854738,0.65600009450625,0.694767121663667),
 .UNSPECIFIED.);
#342=B_SPLINE_CURVE_WITH_KNOTS('',3,(#11375,#11376,#11377,#11378,#11379,
#11380,#11381,#11382,#11383,#11384,#11385,#11386,#11387,#11388,#11389,#11390,
#11391,#11392,#11393,#11394,#11395,#11396),.UNSPECIFIED.,.F.,.F.,(4,2,2,
2,2,2,2,2,2,2,4),(0.0464897534940957,0.0852567806515119,0.170513561303024,
0.246687263103517,0.308657850341199,0.370628437578881,0.432599024816563,
0.494569612054245,0.570743313854738,0.65600009450625,0.694767121663666),
 .UNSPECIFIED.);
#343=B_SPLINE_CURVE_WITH_KNOTS('',3,(#11400,#11401,#11402,#11403,#11404,
#11405,#11406,#11407,#11408,#11409,#11410,#11411,#11412,#11413,#11414,#11415,
#11416,#11417,#11418,#11419,#11420,#11421),.UNSPECIFIED.,.F.,.F.,(4,2,2,
2,2,2,2,2,2,2,4),(0.0464897534940957,0.0852567806515119,0.170513561303024,
0.246687263103517,0.308657850341199,0.370628437578881,0.432599024816563,
0.494569612054245,0.570743313854739,0.656000094506251,0.694767121663667),
 .UNSPECIFIED.);
#344=B_SPLINE_CURVE_WITH_KNOTS('',3,(#11429,#11430,#11431,#11432,#11433,
#11434,#11435,#11436,#11437,#11438,#11439,#11440,#11441,#11442,#11443,#11444,
#11445,#11446,#11447,#11448,#11449,#11450),.UNSPECIFIED.,.F.,.F.,(4,2,2,
2,2,2,2,2,2,2,4),(0.0473477652366656,0.126350602536658,0.189525903804987,
0.252701205073316,0.313298422430274,0.373895639787232,0.434492857144191,
0.495090074501149,0.558265375769478,0.621440677037807,0.7004435143378),
 .UNSPECIFIED.);
#345=B_SPLINE_CURVE_WITH_KNOTS('',3,(#11458,#11459,#11460,#11461,#11462,
#11463,#11464,#11465,#11466,#11467,#11468,#11469,#11470,#11471,#11472,#11473,
#11474,#11475,#11476,#11477,#11478,#11479),.UNSPECIFIED.,.F.,.F.,(4,2,2,
2,2,2,2,2,2,2,4),(0.0473477652366656,0.126350602536658,0.189525903804987,
0.252701205073317,0.313298422430275,0.373895639787233,0.434492857144191,
0.495090074501149,0.558265375769478,0.621440677037807,0.7004435143378),
 .UNSPECIFIED.);
#346=B_SPLINE_CURVE_WITH_KNOTS('',3,(#11488,#11489,#11490,#11491,#11492,
#11493,#11494,#11495,#11496,#11497,#11498,#11499),.UNSPECIFIED.,.F.,.F.,
(4,2,2,2,2,4),(0.0473477652366656,0.126350602536658,0.189525903804987,0.252701205073316,
0.313298422430275,0.373895639787233),.UNSPECIFIED.);
#347=B_SPLINE_CURVE_WITH_KNOTS('',3,(#11501,#11502,#11503,#11504,#11505,
#11506,#11507,#11508,#11509,#11510,#11511,#11512),.UNSPECIFIED.,.F.,.F.,
(4,2,2,2,2,4),(0.373895639787233,0.434492857144191,0.495090074501149,0.558265375769478,
0.621440677037807,0.7004435143378),.UNSPECIFIED.);
#348=B_SPLINE_CURVE_WITH_KNOTS('',3,(#11519,#11520,#11521,#11522,#11523,
#11524,#11525,#11526,#11527,#11528,#11529,#11530,#11531,#11532,#11533,#11534,
#11535,#11536,#11537,#11538,#11539,#11540),.UNSPECIFIED.,.F.,.F.,(4,2,2,
2,2,2,2,2,2,2,4),(0.0473477652366656,0.126350602536658,0.189525903804987,
0.252701205073316,0.313298422430275,0.373895639787233,0.434492857144191,
0.495090074501149,0.558265375769478,0.621440677037807,0.7004435143378),
 .UNSPECIFIED.);
#349=B_SPLINE_CURVE_WITH_KNOTS('',3,(#11548,#11549,#11550,#11551,#11552,
#11553,#11554,#11555,#11556,#11557,#11558,#11559,#11560,#11561,#11562,#11563,
#11564,#11565,#11566,#11567,#11568,#11569),.UNSPECIFIED.,.F.,.F.,(4,2,2,
2,2,2,2,2,2,2,4),(0.0473477652366656,0.126350602536658,0.189525903804987,
0.252701205073317,0.313298422430275,0.373895639787233,0.434492857144191,
0.495090074501149,0.558265375769478,0.621440677037807,0.7004435143378),
 .UNSPECIFIED.);
#350=B_SPLINE_CURVE_WITH_KNOTS('',3,(#11577,#11578,#11579,#11580,#11581,
#11582,#11583,#11584,#11585,#11586,#11587,#11588,#11589,#11590,#11591,#11592,
#11593,#11594,#11595,#11596,#11597,#11598),.UNSPECIFIED.,.F.,.F.,(4,2,2,
2,2,2,2,2,2,2,4),(0.0473477652366656,0.126350602536658,0.189525903804987,
0.252701205073316,0.313298422430275,0.373895639787233,0.434492857144191,
0.495090074501149,0.558265375769478,0.621440677037807,0.7004435143378),
 .UNSPECIFIED.);
#351=B_SPLINE_CURVE_WITH_KNOTS('',3,(#11607,#11608,#11609,#11610,#11611,
#11612,#11613,#11614,#11615,#11616,#11617,#11618,#11619,#11620,#11621,#11622,
#11623,#11624,#11625,#11626,#11627,#11628),.UNSPECIFIED.,.F.,.F.,(4,2,2,
2,2,2,2,2,2,2,4),(0.0473477652366656,0.126350602536658,0.189525903804987,
0.252701205073317,0.313298422430275,0.373895639787233,0.434492857144191,
0.495090074501149,0.558265375769478,0.621440677037807,0.7004435143378),
 .UNSPECIFIED.);
#352=B_SPLINE_CURVE_WITH_KNOTS('',3,(#11799,#11800,#11801,#11802,#11803,
#11804,#11805,#11806,#11807,#11808,#11809,#11810,#11811,#11812),
 .UNSPECIFIED.,.F.,.F.,(4,2,2,2,2,2,4),(0.618551524396289,0.626563103102765,
0.689203386094988,0.751843669087211,0.814483952079434,0.877124235071657,
0.885135813778134),.UNSPECIFIED.);
#353=B_SPLINE_CURVE_WITH_KNOTS('',3,(#11816,#11817,#11818,#11819,#11820,
#11821,#11822,#11823),.UNSPECIFIED.,.F.,.F.,(4,2,2,4),(0.250614556362404,
0.313254839354627,0.37589512234685,0.383906701053325),.UNSPECIFIED.);
#354=B_SPLINE_CURVE_WITH_KNOTS('',3,(#11827,#11828,#11829,#11830,#11831,
#11832,#11833,#11834,#11835,#11836,#11837,#11838,#11839,#11840,#11841,#11842,
#11843,#11844,#11845,#11846,#11847,#11848,#11849,#11850,#11851,#11852),
 .UNSPECIFIED.,.F.,.F.,(4,2,2,2,2,2,2,2,2,2,2,2,4),(0.,0.0623062782223143,
0.124612556444629,0.186916384615149,0.249220212785669,0.31152404095619,
0.37382786912671,0.436134147349024,0.498440425571339,0.560746703793653,
0.623052982015967,0.685356810186488,0.747660638357008),.UNSPECIFIED.);
#355=B_SPLINE_CURVE_WITH_KNOTS('',3,(#11853,#11854,#11855,#11856,#11857,
#11858,#11859,#11860,#11861,#11862),.UNSPECIFIED.,.F.,.F.,(4,2,2,2,4),(0.747660638357008,
0.809964466527529,0.872268294698049,0.934574572920363,0.996880851142677),
 .UNSPECIFIED.);
#356=B_SPLINE_CURVE_WITH_KNOTS('',3,(#11863,#11864,#11865,#11866,#11867,
#11868,#11869,#11870),.UNSPECIFIED.,.F.,.F.,(4,2,2,4),(0.117322411671483,
0.125333990377958,0.187974273370181,0.250614556362404),.UNSPECIFIED.);
#357=B_SPLINE_CURVE_WITH_KNOTS('',3,(#12023,#12024,#12025,#12026,#12027,
#12028,#12029,#12030,#12031,#12032),.UNSPECIFIED.,.F.,.F.,(4,2,2,2,4),(0.566550474129931,
0.613761886174531,0.66097329821913,0.708186965196186,0.755400632173242),
 .UNSPECIFIED.);
#358=B_SPLINE_CURVE_WITH_KNOTS('',3,(#12034,#12035,#12036,#12037,#12038,
#12039,#12040,#12041,#12042,#12043,#12044,#12045,#12046,#12047,#12048,#12049,
#12050,#12051),.UNSPECIFIED.,.F.,.F.,(4,2,2,2,2,2,2,2,4),(0.18885015804331,
0.23606157008791,0.283272982132509,0.330486649109565,0.377700316086621,
0.424913983063677,0.472127650040732,0.519339062085332,0.566550474129931),
 .UNSPECIFIED.);
#359=B_SPLINE_CURVE_WITH_KNOTS('',3,(#12052,#12053,#12054,#12055,#12056,
#12057,#12058,#12059,#12060,#12061),.UNSPECIFIED.,.F.,.F.,(4,2,2,2,4),(0.755400632173242,
0.802614299150298,0.849827966127353,0.897039378171953,0.944250790216552),
 .UNSPECIFIED.);
#360=B_SPLINE_CURVE_WITH_KNOTS('',3,(#12065,#12066,#12067,#12068,#12069,
#12070,#12071,#12072,#12073,#12074),.UNSPECIFIED.,.F.,.F.,(4,2,2,2,4),(0.189723673274825,
0.237146208024627,0.28456874277443,0.33200804466204,0.37944734654965),
 .UNSPECIFIED.);
#361=B_SPLINE_CURVE_WITH_KNOTS('',3,(#12076,#12077,#12078,#12079,#12080,
#12081,#12082,#12083,#12084,#12085),.UNSPECIFIED.,.F.,.F.,(4,2,2,2,4),(0.,
0.0474393018876097,0.0948786037752193,0.142301138525022,0.189723673274825),
 .UNSPECIFIED.);
#362=B_SPLINE_CURVE_WITH_KNOTS('',3,(#12087,#12088,#12089,#12090,#12091,
#12092,#12093,#12094,#12095,#12096),.UNSPECIFIED.,.F.,.F.,(4,2,2,2,4),(0.569171019824474,
0.616593554574277,0.66401608932408,0.711455391211689,0.758894693099299),
 .UNSPECIFIED.);
#363=B_SPLINE_CURVE_WITH_KNOTS('',3,(#12097,#12098,#12099,#12100,#12101,
#12102,#12103,#12104,#12105,#12106),.UNSPECIFIED.,.F.,.F.,(4,2,2,2,4),(0.37944734654965,
0.426886648437259,0.474325950324869,0.521748485074671,0.569171019824474),
 .UNSPECIFIED.);
#364=B_SPLINE_CURVE_WITH_KNOTS('',3,(#12110,#12111,#12112,#12113,#12114,
#12115,#12116,#12117,#12118,#12119,#12120,#12121,#12122,#12123,#12124,#12125,
#12126,#12127),.UNSPECIFIED.,.F.,.F.,(4,2,2,2,2,2,2,2,4),(0.,0.0474393018876097,
0.0948786037752194,0.142301138525022,0.189723673274825,0.237146208024628,
0.28456874277443,0.33200804466204,0.37944734654965),.UNSPECIFIED.);
#365=B_SPLINE_CURVE_WITH_KNOTS('',3,(#12128,#12129,#12130,#12131,#12132,
#12133,#12134,#12135,#12136,#12137,#12138,#12139,#12140,#12141,#12142,#12143,
#12144,#12145),.UNSPECIFIED.,.F.,.F.,(4,2,2,2,2,2,2,2,4),(0.37944734654965,
0.426886648437259,0.474325950324869,0.521748485074672,0.569171019824474,
0.616593554574277,0.66401608932408,0.711455391211689,0.758894693099299),
 .UNSPECIFIED.);
#366=B_SPLINE_CURVE_WITH_KNOTS('',3,(#12149,#12150,#12151,#12152,#12153,
#12154,#12155,#12156,#12157,#12158),.UNSPECIFIED.,.F.,.F.,(4,2,2,2,4),(0.566550474129931,
0.613761886174531,0.66097329821913,0.708186965196186,0.755400632173242),
 .UNSPECIFIED.);
#367=B_SPLINE_CURVE_WITH_KNOTS('',3,(#12160,#12161,#12162,#12163,#12164,
#12165,#12166,#12167,#12168,#12169,#12170,#12171,#12172,#12173,#12174,#12175,
#12176,#12177),.UNSPECIFIED.,.F.,.F.,(4,2,2,2,2,2,2,2,4),(0.188850158043311,
0.23606157008791,0.283272982132509,0.330486649109565,0.377700316086621,
0.424913983063677,0.472127650040733,0.519339062085332,0.566550474129931),
 .UNSPECIFIED.);
#368=B_SPLINE_CURVE_WITH_KNOTS('',3,(#12178,#12179,#12180,#12181,#12182,
#12183,#12184,#12185,#12186,#12187),.UNSPECIFIED.,.F.,.F.,(4,2,2,2,4),(0.755400632173242,
0.802614299150298,0.849827966127354,0.897039378171953,0.944250790216552),
 .UNSPECIFIED.);
#369=B_SPLINE_CURVE_WITH_KNOTS('',3,(#12197,#12198,#12199,#12200,#12201,
#12202,#12203,#12204,#12205,#12206,#12207,#12208,#12209,#12210,#12211,#12212,
#12213,#12214),.UNSPECIFIED.,.F.,.F.,(4,2,2,2,2,2,2,2,4),(0.18885015804331,
0.23606157008791,0.283272982132509,0.330486649109565,0.377700316086621,
0.424913983063677,0.472127650040732,0.519339062085332,0.566550474129931),
 .UNSPECIFIED.);
#370=B_SPLINE_CURVE_WITH_KNOTS('',3,(#12216,#12217,#12218,#12219,#12220,
#12221,#12222,#12223,#12224,#12225),.UNSPECIFIED.,.F.,.F.,(4,2,2,2,4),(0.566550474129931,
0.613761886174531,0.66097329821913,0.708186965196186,0.755400632173242),
 .UNSPECIFIED.);
#371=B_SPLINE_CURVE_WITH_KNOTS('',3,(#12226,#12227,#12228,#12229,#12230,
#12231,#12232,#12233,#12234,#12235),.UNSPECIFIED.,.F.,.F.,(4,2,2,2,4),(0.755400632173242,
0.802614299150298,0.849827966127353,0.897039378171953,0.944250790216552),
 .UNSPECIFIED.);
#372=B_SPLINE_CURVE_WITH_KNOTS('',3,(#12238,#12239,#12240,#12241,#12242,
#12243,#12244,#12245,#12246,#12247,#12248,#12249,#12250,#12251,#12252,#12253,
#12254,#12255),.UNSPECIFIED.,.F.,.F.,(4,2,2,2,2,2,2,2,4),(0.188850158043311,
0.23606157008791,0.283272982132509,0.330486649109565,0.377700316086621,
0.424913983063677,0.472127650040733,0.519339062085332,0.566550474129932),
 .UNSPECIFIED.);
#373=B_SPLINE_CURVE_WITH_KNOTS('',3,(#12257,#12258,#12259,#12260,#12261,
#12262,#12263,#12264,#12265,#12266),.UNSPECIFIED.,.F.,.F.,(4,2,2,2,4),(0.566550474129932,
0.613761886174531,0.66097329821913,0.708186965196186,0.755400632173242),
 .UNSPECIFIED.);
#374=B_SPLINE_CURVE_WITH_KNOTS('',3,(#12267,#12268,#12269,#12270,#12271,
#12272,#12273,#12274,#12275,#12276),.UNSPECIFIED.,.F.,.F.,(4,2,2,2,4),(0.755400632173242,
0.802614299150298,0.849827966127354,0.897039378171953,0.944250790216552),
 .UNSPECIFIED.);
#375=B_SPLINE_CURVE_WITH_KNOTS('',3,(#12281,#12282,#12283,#12284,#12285,
#12286,#12287,#12288,#12289,#12290,#12291,#12292,#12293,#12294,#12295,#12296,
#12297,#12298),.UNSPECIFIED.,.F.,.F.,(4,2,2,2,2,2,2,2,4),(0.,0.0474393018876097,
0.0948786037752193,0.142301138525022,0.189723673274825,0.237146208024627,
0.28456874277443,0.33200804466204,0.37944734654965),.UNSPECIFIED.);
#376=B_SPLINE_CURVE_WITH_KNOTS('',3,(#12299,#12300,#12301,#12302,#12303,
#12304,#12305,#12306,#12307,#12308,#12309,#12310,#12311,#12312,#12313,#12314,
#12315,#12316),.UNSPECIFIED.,.F.,.F.,(4,2,2,2,2,2,2,2,4),(0.37944734654965,
0.426886648437259,0.474325950324869,0.521748485074672,0.569171019824474,
0.616593554574277,0.66401608932408,0.711455391211689,0.758894693099299),
 .UNSPECIFIED.);
#377=B_SPLINE_CURVE_WITH_KNOTS('',3,(#12320,#12321,#12322,#12323,#12324,
#12325,#12326,#12327,#12328,#12329,#12330,#12331,#12332,#12333,#12334,#12335,
#12336,#12337),.UNSPECIFIED.,.F.,.F.,(4,2,2,2,2,2,2,2,4),(0.,0.0474393018876097,
0.0948786037752194,0.142301138525022,0.189723673274825,0.237146208024627,
0.28456874277443,0.33200804466204,0.37944734654965),.UNSPECIFIED.);
#378=B_SPLINE_CURVE_WITH_KNOTS('',3,(#12338,#12339,#12340,#12341,#12342,
#12343,#12344,#12345,#12346,#12347,#12348,#12349,#12350,#12351,#12352,#12353,
#12354,#12355),.UNSPECIFIED.,.F.,.F.,(4,2,2,2,2,2,2,2,4),(0.37944734654965,
0.426886648437259,0.474325950324869,0.521748485074672,0.569171019824474,
0.616593554574277,0.66401608932408,0.711455391211689,0.758894693099299),
 .UNSPECIFIED.);
#379=SHAPE_REPRESENTATION_RELATIONSHIP('SRR','None',#12925,#413);
#380=SHAPE_REPRESENTATION_RELATIONSHIP('SRR','None',#12926,#414);
#381=SHAPE_REPRESENTATION_RELATIONSHIP('SRR','None',#12927,#415);
#382=SHAPE_REPRESENTATION_RELATIONSHIP('SRR','None',#12928,#416);
#383=SHAPE_REPRESENTATION_RELATIONSHIP('SRR','None',#12929,#417);
#384=SHAPE_REPRESENTATION_RELATIONSHIP('SRR','None',#12930,#418);
#385=SHAPE_REPRESENTATION_RELATIONSHIP('SRR','None',#12931,#419);
#386=SHAPE_REPRESENTATION_RELATIONSHIP('SRR','None',#12932,#420);
#387=SHAPE_REPRESENTATION_RELATIONSHIP('SRR','None',#12933,#421);
#388=SHAPE_REPRESENTATION_RELATIONSHIP('SRR','None',#12934,#422);
#389=SHAPE_REPRESENTATION_RELATIONSHIP('SRR','None',#12935,#423);
#390=SHAPE_REPRESENTATION_RELATIONSHIP('SRR','None',#12936,#424);
#391=SHAPE_REPRESENTATION_RELATIONSHIP('SRR','None',#12938,#425);
#392=SHAPE_REPRESENTATION_RELATIONSHIP('SRR','None',#12939,#426);
#393=SHAPE_REPRESENTATION_RELATIONSHIP('SRR','None',#12940,#427);
#394=SHAPE_REPRESENTATION_RELATIONSHIP('SRR','None',#12941,#428);
#395=SHAPE_REPRESENTATION_RELATIONSHIP('SRR','None',#12942,#429);
#396=SHAPE_REPRESENTATION_RELATIONSHIP('SRR','None',#12943,#430);
#397=SHAPE_REPRESENTATION_RELATIONSHIP('SRR','None',#12945,#431);
#398=SHAPE_REPRESENTATION_RELATIONSHIP('SRR','None',#12946,#432);
#399=SHAPE_REPRESENTATION_RELATIONSHIP('SRR','None',#12947,#433);
#400=SHAPE_REPRESENTATION_RELATIONSHIP('SRR','None',#12948,#434);
#401=SHAPE_REPRESENTATION_RELATIONSHIP('SRR','None',#12949,#435);
#402=SHAPE_REPRESENTATION_RELATIONSHIP('SRR','None',#12950,#436);
#403=SHAPE_REPRESENTATION_RELATIONSHIP('SRR','None',#12952,#437);
#404=SHAPE_REPRESENTATION_RELATIONSHIP('SRR','None',#12953,#438);
#405=SHAPE_REPRESENTATION_RELATIONSHIP('SRR','None',#12954,#439);
#406=SHAPE_REPRESENTATION_RELATIONSHIP('SRR','None',#12955,#440);
#407=SHAPE_REPRESENTATION_RELATIONSHIP('SRR','None',#12956,#441);
#408=SHAPE_REPRESENTATION_RELATIONSHIP('SRR','None',#12957,#442);
#409=SHAPE_REPRESENTATION_RELATIONSHIP('SRR','None',#12958,#443);
#410=SHAPE_REPRESENTATION_RELATIONSHIP('SRR','None',#12959,#444);
#411=SHAPE_REPRESENTATION_RELATIONSHIP('SRR','None',#12960,#445);
#412=SHAPE_REPRESENTATION_RELATIONSHIP('SRR','None',#12961,#446);
#413=ADVANCED_BREP_SHAPE_REPRESENTATION('',(#489),#12742);
#414=ADVANCED_BREP_SHAPE_REPRESENTATION('',(#490),#12743);
#415=ADVANCED_BREP_SHAPE_REPRESENTATION('',(#491),#12744);
#416=ADVANCED_BREP_SHAPE_REPRESENTATION('',(#492),#12745);
#417=ADVANCED_BREP_SHAPE_REPRESENTATION('',(#493),#12746);
#418=ADVANCED_BREP_SHAPE_REPRESENTATION('',(#494),#12747);
#419=ADVANCED_BREP_SHAPE_REPRESENTATION('',(#495),#12748);
#420=ADVANCED_BREP_SHAPE_REPRESENTATION('',(#496),#12749);
#421=ADVANCED_BREP_SHAPE_REPRESENTATION('',(#497),#12750);
#422=ADVANCED_BREP_SHAPE_REPRESENTATION('',(#289),#12751);
#423=ADVANCED_BREP_SHAPE_REPRESENTATION('',(#498),#12752);
#424=ADVANCED_BREP_SHAPE_REPRESENTATION('',(#290),#12753);
#425=ADVANCED_BREP_SHAPE_REPRESENTATION('',(#499),#12755);
#426=ADVANCED_BREP_SHAPE_REPRESENTATION('',(#500),#12756);
#427=ADVANCED_BREP_SHAPE_REPRESENTATION('',(#501),#12757);
#428=ADVANCED_BREP_SHAPE_REPRESENTATION('',(#502),#12758);
#429=ADVANCED_BREP_SHAPE_REPRESENTATION('',(#503),#12759);
#430=ADVANCED_BREP_SHAPE_REPRESENTATION('',(#504),#12760);
#431=ADVANCED_BREP_SHAPE_REPRESENTATION('',(#505),#12762);
#432=ADVANCED_BREP_SHAPE_REPRESENTATION('',(#506),#12763);
#433=ADVANCED_BREP_SHAPE_REPRESENTATION('',(#507,#508,#509,#510,#511,#512,
#513,#514),#12764);
#434=ADVANCED_BREP_SHAPE_REPRESENTATION('',(#515),#12765);
#435=ADVANCED_BREP_SHAPE_REPRESENTATION('',(#516,#517),#12766);
#436=ADVANCED_BREP_SHAPE_REPRESENTATION('',(#291),#12767);
#437=ADVANCED_BREP_SHAPE_REPRESENTATION('',(#518),#12769);
#438=ADVANCED_BREP_SHAPE_REPRESENTATION('',(#519),#12770);
#439=ADVANCED_BREP_SHAPE_REPRESENTATION('',(#520),#12771);
#440=ADVANCED_BREP_SHAPE_REPRESENTATION('',(#521),#12772);
#441=ADVANCED_BREP_SHAPE_REPRESENTATION('',(#522),#12773);
#442=ADVANCED_BREP_SHAPE_REPRESENTATION('',(#523),#12774);
#443=ADVANCED_BREP_SHAPE_REPRESENTATION('',(#524),#12775);
#444=ADVANCED_BREP_SHAPE_REPRESENTATION('',(#525),#12776);
#445=ADVANCED_BREP_SHAPE_REPRESENTATION('',(#526),#12777);
#446=ADVANCED_BREP_SHAPE_REPRESENTATION('',(#292),#12778);
#447=STYLED_ITEM('',(#13163),#489);
#448=STYLED_ITEM('',(#13198),#490);
#449=STYLED_ITEM('',(#13198),#491);
#450=STYLED_ITEM('',(#13184),#492);
#451=STYLED_ITEM('',(#13170),#493);
#452=STYLED_ITEM('',(#13184),#494);
#453=STYLED_ITEM('',(#13184),#495);
#454=STYLED_ITEM('',(#13191),#496);
#455=STYLED_ITEM('',(#13191),#497);
#456=STYLED_ITEM('',(#13191),#289);
#457=STYLED_ITEM('',(#13191),#498);
#458=STYLED_ITEM('',(#13191),#290);
#459=STYLED_ITEM('',(#13177),#499);
#460=STYLED_ITEM('',(#13184),#500);
#461=STYLED_ITEM('',(#13184),#501);
#462=STYLED_ITEM('',(#13184),#502);
#463=STYLED_ITEM('',(#13184),#503);
#464=STYLED_ITEM('',(#13184),#504);
#465=STYLED_ITEM('',(#13184),#505);
#466=STYLED_ITEM('',(#13184),#506);
#467=STYLED_ITEM('',(#13184),#507);
#468=STYLED_ITEM('',(#13184),#508);
#469=STYLED_ITEM('',(#13184),#509);
#470=STYLED_ITEM('',(#13184),#510);
#471=STYLED_ITEM('',(#13184),#511);
#472=STYLED_ITEM('',(#13184),#512);
#473=STYLED_ITEM('',(#13184),#513);
#474=STYLED_ITEM('',(#13184),#514);
#475=STYLED_ITEM('',(#13184),#515);
#476=STYLED_ITEM('',(#13184),#516);
#477=STYLED_ITEM('',(#13184),#517);
#478=STYLED_ITEM('',(#13191),#291);
#479=STYLED_ITEM('',(#13184),#518);
#480=STYLED_ITEM('',(#13177),#519);
#481=STYLED_ITEM('',(#13177),#520);
#482=STYLED_ITEM('',(#13170),#521);
#483=STYLED_ITEM('',(#13191),#522);
#484=STYLED_ITEM('',(#13191),#523);
#485=STYLED_ITEM('',(#13184),#524);
#486=STYLED_ITEM('',(#13191),#525);
#487=STYLED_ITEM('',(#13198),#526);
#488=STYLED_ITEM('',(#13191),#292);
#489=MANIFOLD_SOLID_BREP('Body1',#6181);
#490=MANIFOLD_SOLID_BREP('Body1',#6182);
#491=MANIFOLD_SOLID_BREP('Body1',#6183);
#492=MANIFOLD_SOLID_BREP('Body1',#6184);
#493=MANIFOLD_SOLID_BREP('Body1',#6185);
#494=MANIFOLD_SOLID_BREP('Body1',#6186);
#495=MANIFOLD_SOLID_BREP('Body1',#6187);
#496=MANIFOLD_SOLID_BREP('Body1',#6188);
#497=MANIFOLD_SOLID_BREP('Body1',#6189);
#498=MANIFOLD_SOLID_BREP('Body1',#6192);
#499=MANIFOLD_SOLID_BREP('Body1',#6195);
#500=MANIFOLD_SOLID_BREP('Body1',#6196);
#501=MANIFOLD_SOLID_BREP('Body1',#6197);
#502=MANIFOLD_SOLID_BREP('Body1',#6198);
#503=MANIFOLD_SOLID_BREP('Body1',#6199);
#504=MANIFOLD_SOLID_BREP('Body1',#6200);
#505=MANIFOLD_SOLID_BREP('Body1',#6201);
#506=MANIFOLD_SOLID_BREP('Body1',#6202);
#507=MANIFOLD_SOLID_BREP('Body1',#6203);
#508=MANIFOLD_SOLID_BREP('Body2',#6204);
#509=MANIFOLD_SOLID_BREP('Body3',#6205);
#510=MANIFOLD_SOLID_BREP('Body4',#6206);
#511=MANIFOLD_SOLID_BREP('Body5',#6207);
#512=MANIFOLD_SOLID_BREP('Body6',#6208);
#513=MANIFOLD_SOLID_BREP('Body7',#6209);
#514=MANIFOLD_SOLID_BREP('Body8',#6210);
#515=MANIFOLD_SOLID_BREP('Continuous crown cage',#6211);
#516=MANIFOLD_SOLID_BREP('Body1',#6212);
#517=MANIFOLD_SOLID_BREP('Body2',#6213);
#518=MANIFOLD_SOLID_BREP('Body1',#6216);
#519=MANIFOLD_SOLID_BREP('Body1',#6217);
#520=MANIFOLD_SOLID_BREP('Body1',#6218);
#521=MANIFOLD_SOLID_BREP('Body1',#6219);
#522=MANIFOLD_SOLID_BREP('Body1',#6220);
#523=MANIFOLD_SOLID_BREP('Body1',#6221);
#524=MANIFOLD_SOLID_BREP('Body1',#6222);
#525=MANIFOLD_SOLID_BREP('Body1',#6223);
#526=MANIFOLD_SOLID_BREP('Body1',#6224);
#527=FACE_BOUND('',#1214,.T.);
#528=FACE_BOUND('',#1215,.T.);
#529=FACE_BOUND('',#1216,.T.);
#530=FACE_BOUND('',#1217,.T.);
#531=FACE_BOUND('',#1218,.T.);
#532=FACE_BOUND('',#1220,.T.);
#533=FACE_BOUND('',#1221,.T.);
#534=FACE_BOUND('',#1222,.T.);
#535=FACE_BOUND('',#1223,.T.);
#536=FACE_BOUND('',#1224,.T.);
#537=FACE_BOUND('',#1241,.T.);
#538=FACE_BOUND('',#1246,.T.);
#539=FACE_BOUND('',#1247,.T.);
#540=FACE_BOUND('',#1248,.T.);
#541=FACE_BOUND('',#1249,.T.);
#542=FACE_BOUND('',#1253,.T.);
#543=FACE_BOUND('',#1255,.T.);
#544=FACE_BOUND('',#1256,.T.);
#545=FACE_BOUND('',#1257,.T.);
#546=FACE_BOUND('',#1262,.T.);
#547=FACE_BOUND('',#1264,.T.);
#548=FACE_BOUND('',#1266,.T.);
#549=FACE_BOUND('',#1268,.T.);
#550=FACE_BOUND('',#1273,.T.);
#551=FACE_BOUND('',#1274,.T.);
#552=FACE_BOUND('',#1277,.T.);
#553=FACE_BOUND('',#1294,.T.);
#554=FACE_BOUND('',#1297,.T.);
#555=FACE_BOUND('',#1301,.T.);
#556=FACE_BOUND('',#1305,.T.);
#557=FACE_BOUND('',#1308,.T.);
#558=FACE_BOUND('',#1314,.T.);
#559=FACE_BOUND('',#1337,.T.);
#560=FACE_BOUND('',#1339,.T.);
#561=FACE_BOUND('',#1345,.T.);
#562=FACE_BOUND('',#1371,.T.);
#563=FACE_BOUND('',#1372,.T.);
#564=FACE_BOUND('',#1373,.T.);
#565=FACE_BOUND('',#1374,.T.);
#566=FACE_BOUND('',#1375,.T.);
#567=FACE_BOUND('',#1376,.T.);
#568=FACE_BOUND('',#1377,.T.);
#569=FACE_BOUND('',#1378,.T.);
#570=FACE_BOUND('',#1379,.T.);
#571=FACE_BOUND('',#1380,.T.);
#572=FACE_BOUND('',#1384,.T.);
#573=FACE_BOUND('',#1385,.T.);
#574=FACE_BOUND('',#1386,.T.);
#575=FACE_BOUND('',#1387,.T.);
#576=FACE_BOUND('',#1388,.T.);
#577=FACE_BOUND('',#1389,.T.);
#578=FACE_BOUND('',#1390,.T.);
#579=FACE_BOUND('',#1391,.T.);
#580=FACE_BOUND('',#1392,.T.);
#581=FACE_BOUND('',#1393,.T.);
#582=FACE_BOUND('',#1400,.T.);
#583=FACE_BOUND('',#1404,.T.);
#584=FACE_BOUND('',#1405,.T.);
#585=FACE_BOUND('',#1406,.T.);
#586=FACE_BOUND('',#1407,.T.);
#587=FACE_BOUND('',#1408,.T.);
#588=FACE_BOUND('',#1410,.T.);
#589=FACE_BOUND('',#1411,.T.);
#590=FACE_BOUND('',#1412,.T.);
#591=FACE_BOUND('',#1413,.T.);
#592=FACE_BOUND('',#1414,.T.);
#593=FACE_BOUND('',#1421,.T.);
#594=FACE_BOUND('',#1425,.T.);
#595=FACE_BOUND('',#1426,.T.);
#596=FACE_BOUND('',#1427,.T.);
#597=FACE_BOUND('',#1428,.T.);
#598=FACE_BOUND('',#1429,.T.);
#599=FACE_BOUND('',#1431,.T.);
#600=FACE_BOUND('',#1432,.T.);
#601=FACE_BOUND('',#1433,.T.);
#602=FACE_BOUND('',#1434,.T.);
#603=FACE_BOUND('',#1435,.T.);
#604=FACE_BOUND('',#1442,.T.);
#605=FACE_BOUND('',#1446,.T.);
#606=FACE_BOUND('',#1447,.T.);
#607=FACE_BOUND('',#1448,.T.);
#608=FACE_BOUND('',#1449,.T.);
#609=FACE_BOUND('',#1450,.T.);
#610=FACE_BOUND('',#1452,.T.);
#611=FACE_BOUND('',#1453,.T.);
#612=FACE_BOUND('',#1454,.T.);
#613=FACE_BOUND('',#1455,.T.);
#614=FACE_BOUND('',#1456,.T.);
#615=FACE_BOUND('',#1463,.T.);
#616=FACE_BOUND('',#1467,.T.);
#617=FACE_BOUND('',#1468,.T.);
#618=FACE_BOUND('',#1469,.T.);
#619=FACE_BOUND('',#1470,.T.);
#620=FACE_BOUND('',#1471,.T.);
#621=FACE_BOUND('',#1473,.T.);
#622=FACE_BOUND('',#1474,.T.);
#623=FACE_BOUND('',#1475,.T.);
#624=FACE_BOUND('',#1476,.T.);
#625=FACE_BOUND('',#1477,.T.);
#626=FACE_BOUND('',#1480,.T.);
#627=FACE_BOUND('',#1495,.T.);
#628=FACE_BOUND('',#1498,.T.);
#629=FACE_BOUND('',#1503,.T.);
#630=FACE_BOUND('',#1508,.T.);
#631=FACE_BOUND('',#1536,.T.);
#632=FACE_BOUND('',#1539,.T.);
#633=FACE_BOUND('',#1542,.T.);
#634=FACE_BOUND('',#1545,.T.);
#635=FACE_BOUND('',#1548,.T.);
#636=FACE_BOUND('',#1556,.T.);
#637=FACE_BOUND('',#1571,.T.);
#638=FACE_BOUND('',#1573,.T.);
#639=FACE_BOUND('',#1577,.T.);
#640=FACE_BOUND('',#1583,.T.);
#641=FACE_BOUND('',#1585,.T.);
#642=FACE_BOUND('',#1587,.T.);
#643=FACE_BOUND('',#1589,.T.);
#644=FACE_BOUND('',#1593,.T.);
#645=FACE_BOUND('',#1595,.T.);
#646=FACE_BOUND('',#1599,.T.);
#647=FACE_BOUND('',#1601,.T.);
#648=FACE_BOUND('',#1611,.T.);
#649=FACE_BOUND('',#1613,.T.);
#650=FACE_BOUND('',#1623,.T.);
#651=FACE_BOUND('',#1629,.T.);
#652=FACE_BOUND('',#1630,.T.);
#653=FACE_BOUND('',#1631,.T.);
#654=FACE_BOUND('',#1635,.T.);
#655=FACE_BOUND('',#1636,.T.);
#656=FACE_BOUND('',#1637,.T.);
#657=FACE_BOUND('',#1639,.T.);
#658=FACE_BOUND('',#1641,.T.);
#659=FACE_BOUND('',#1644,.T.);
#660=FACE_BOUND('',#1646,.T.);
#661=FACE_BOUND('',#1649,.T.);
#662=FACE_BOUND('',#1704,.T.);
#663=PLANE('',#6620);
#664=PLANE('',#6621);
#665=PLANE('',#6622);
#666=PLANE('',#6623);
#667=PLANE('',#6624);
#668=PLANE('',#6625);
#669=PLANE('',#6627);
#670=PLANE('',#6628);
#671=PLANE('',#6629);
#672=PLANE('',#6630);
#673=PLANE('',#6631);
#674=PLANE('',#6632);
#675=PLANE('',#6634);
#676=PLANE('',#6635);
#677=PLANE('',#6636);
#678=PLANE('',#6637);
#679=PLANE('',#6638);
#680=PLANE('',#6639);
#681=PLANE('',#6650);
#682=PLANE('',#6657);
#683=PLANE('',#6658);
#684=PLANE('',#6665);
#685=PLANE('',#6666);
#686=PLANE('',#6668);
#687=PLANE('',#6672);
#688=PLANE('',#6679);
#689=PLANE('',#6680);
#690=PLANE('',#6685);
#691=PLANE('',#6690);
#692=PLANE('',#6691);
#693=PLANE('',#6697);
#694=PLANE('',#6698);
#695=PLANE('',#6699);
#696=PLANE('',#6704);
#697=PLANE('',#6705);
#698=PLANE('',#6712);
#699=PLANE('',#6713);
#700=PLANE('',#6714);
#701=PLANE('',#6719);
#702=PLANE('',#6723);
#703=PLANE('',#6724);
#704=PLANE('',#6725);
#705=PLANE('',#6726);
#706=PLANE('',#6727);
#707=PLANE('',#6728);
#708=PLANE('',#6735);
#709=PLANE('',#6739);
#710=PLANE('',#6741);
#711=PLANE('',#6749);
#712=PLANE('',#6757);
#713=PLANE('',#6758);
#714=PLANE('',#6759);
#715=PLANE('',#6760);
#716=PLANE('',#6761);
#717=PLANE('',#6762);
#718=PLANE('',#6763);
#719=PLANE('',#6764);
#720=PLANE('',#6765);
#721=PLANE('',#6771);
#722=PLANE('',#6772);
#723=PLANE('',#6773);
#724=PLANE('',#6777);
#725=PLANE('',#6778);
#726=PLANE('',#6779);
#727=PLANE('',#6780);
#728=PLANE('',#6781);
#729=PLANE('',#6783);
#730=PLANE('',#6791);
#731=PLANE('',#6799);
#732=PLANE('',#6800);
#733=PLANE('',#6801);
#734=PLANE('',#6802);
#735=PLANE('',#6803);
#736=PLANE('',#6804);
#737=PLANE('',#6805);
#738=PLANE('',#6806);
#739=PLANE('',#6807);
#740=PLANE('',#6843);
#741=PLANE('',#6844);
#742=PLANE('',#6846);
#743=PLANE('',#6849);
#744=PLANE('',#6866);
#745=PLANE('',#6873);
#746=PLANE('',#6874);
#747=PLANE('',#6891);
#748=PLANE('',#6898);
#749=PLANE('',#6899);
#750=PLANE('',#6916);
#751=PLANE('',#6923);
#752=PLANE('',#6924);
#753=PLANE('',#6941);
#754=PLANE('',#6948);
#755=PLANE('',#6949);
#756=PLANE('',#6957);
#757=PLANE('',#6958);
#758=PLANE('',#6959);
#759=PLANE('',#6960);
#760=PLANE('',#6961);
#761=PLANE('',#6962);
#762=PLANE('',#6963);
#763=PLANE('',#6964);
#764=PLANE('',#6965);
#765=PLANE('',#6981);
#766=PLANE('',#6984);
#767=PLANE('',#6996);
#768=PLANE('',#7005);
#769=PLANE('',#7038);
#770=PLANE('',#7043);
#771=PLANE('',#7048);
#772=PLANE('',#7053);
#773=PLANE('',#7058);
#774=PLANE('',#7063);
#775=PLANE('',#7072);
#776=PLANE('',#7076);
#777=PLANE('',#7077);
#778=PLANE('',#7079);
#779=PLANE('',#7084);
#780=PLANE('',#7087);
#781=PLANE('',#7092);
#782=PLANE('',#7101);
#783=PLANE('',#7103);
#784=PLANE('',#7111);
#785=PLANE('',#7116);
#786=PLANE('',#7117);
#787=PLANE('',#7118);
#788=PLANE('',#7119);
#789=PLANE('',#7120);
#790=PLANE('',#7121);
#791=PLANE('',#7122);
#792=PLANE('',#7123);
#793=PLANE('',#7153);
#794=PLANE('',#7157);
#795=PLANE('',#7158);
#796=PLANE('',#7165);
#797=PLANE('',#7166);
#798=PLANE('',#7168);
#799=PLANE('',#7172);
#800=PLANE('',#7179);
#801=PLANE('',#7180);
#802=PLANE('',#7188);
#803=PLANE('',#7189);
#804=PLANE('',#7197);
#805=PLANE('',#7198);
#806=PLANE('',#7203);
#807=PLANE('',#7204);
#808=PLANE('',#7209);
#809=PLANE('',#7210);
#810=PLANE('',#7218);
#811=PLANE('',#7219);
#812=PLANE('',#7221);
#813=PLANE('',#7223);
#814=PLANE('',#7224);
#815=PLANE('',#7225);
#816=PLANE('',#7226);
#817=PLANE('',#7227);
#818=PLANE('',#7228);
#819=PLANE('',#7229);
#820=PLANE('',#7230);
#821=PLANE('',#7265);
#822=PLANE('',#7266);
#823=PLANE('',#7310);
#824=PLANE('',#7311);
#825=PLANE('',#7355);
#826=PLANE('',#7397);
#827=PLANE('',#7398);
#828=PLANE('',#7399);
#829=PLANE('',#7400);
#830=PLANE('',#7401);
#831=PLANE('',#7402);
#832=PLANE('',#7403);
#833=PLANE('',#7404);
#834=PLANE('',#7405);
#835=PLANE('',#7407);
#836=PLANE('',#7415);
#837=FACE_OUTER_BOUND('',#1204,.T.);
#838=FACE_OUTER_BOUND('',#1205,.T.);
#839=FACE_OUTER_BOUND('',#1206,.T.);
#840=FACE_OUTER_BOUND('',#1207,.T.);
#841=FACE_OUTER_BOUND('',#1208,.T.);
#842=FACE_OUTER_BOUND('',#1209,.T.);
#843=FACE_OUTER_BOUND('',#1210,.T.);
#844=FACE_OUTER_BOUND('',#1211,.T.);
#845=FACE_OUTER_BOUND('',#1212,.T.);
#846=FACE_OUTER_BOUND('',#1213,.T.);
#847=FACE_OUTER_BOUND('',#1219,.T.);
#848=FACE_OUTER_BOUND('',#1225,.T.);
#849=FACE_OUTER_BOUND('',#1226,.T.);
#850=FACE_OUTER_BOUND('',#1227,.T.);
#851=FACE_OUTER_BOUND('',#1228,.T.);
#852=FACE_OUTER_BOUND('',#1229,.T.);
#853=FACE_OUTER_BOUND('',#1230,.T.);
#854=FACE_OUTER_BOUND('',#1231,.T.);
#855=FACE_OUTER_BOUND('',#1232,.T.);
#856=FACE_OUTER_BOUND('',#1233,.T.);
#857=FACE_OUTER_BOUND('',#1234,.T.);
#858=FACE_OUTER_BOUND('',#1235,.T.);
#859=FACE_OUTER_BOUND('',#1236,.T.);
#860=FACE_OUTER_BOUND('',#1237,.T.);
#861=FACE_OUTER_BOUND('',#1238,.T.);
#862=FACE_OUTER_BOUND('',#1239,.T.);
#863=FACE_OUTER_BOUND('',#1240,.T.);
#864=FACE_OUTER_BOUND('',#1242,.T.);
#865=FACE_OUTER_BOUND('',#1243,.T.);
#866=FACE_OUTER_BOUND('',#1244,.T.);
#867=FACE_OUTER_BOUND('',#1245,.T.);
#868=FACE_OUTER_BOUND('',#1250,.T.);
#869=FACE_OUTER_BOUND('',#1251,.T.);
#870=FACE_OUTER_BOUND('',#1252,.T.);
#871=FACE_OUTER_BOUND('',#1254,.T.);
#872=FACE_OUTER_BOUND('',#1258,.T.);
#873=FACE_OUTER_BOUND('',#1259,.T.);
#874=FACE_OUTER_BOUND('',#1260,.T.);
#875=FACE_OUTER_BOUND('',#1261,.T.);
#876=FACE_OUTER_BOUND('',#1263,.T.);
#877=FACE_OUTER_BOUND('',#1265,.T.);
#878=FACE_OUTER_BOUND('',#1267,.T.);
#879=FACE_OUTER_BOUND('',#1269,.T.);
#880=FACE_OUTER_BOUND('',#1270,.T.);
#881=FACE_OUTER_BOUND('',#1271,.T.);
#882=FACE_OUTER_BOUND('',#1272,.T.);
#883=FACE_OUTER_BOUND('',#1275,.T.);
#884=FACE_OUTER_BOUND('',#1276,.T.);
#885=FACE_OUTER_BOUND('',#1278,.T.);
#886=FACE_OUTER_BOUND('',#1279,.T.);
#887=FACE_OUTER_BOUND('',#1280,.T.);
#888=FACE_OUTER_BOUND('',#1281,.T.);
#889=FACE_OUTER_BOUND('',#1282,.T.);
#890=FACE_OUTER_BOUND('',#1283,.T.);
#891=FACE_OUTER_BOUND('',#1284,.T.);
#892=FACE_OUTER_BOUND('',#1285,.T.);
#893=FACE_OUTER_BOUND('',#1286,.T.);
#894=FACE_OUTER_BOUND('',#1287,.T.);
#895=FACE_OUTER_BOUND('',#1288,.T.);
#896=FACE_OUTER_BOUND('',#1289,.T.);
#897=FACE_OUTER_BOUND('',#1290,.T.);
#898=FACE_OUTER_BOUND('',#1291,.T.);
#899=FACE_OUTER_BOUND('',#1292,.T.);
#900=FACE_OUTER_BOUND('',#1293,.T.);
#901=FACE_OUTER_BOUND('',#1295,.T.);
#902=FACE_OUTER_BOUND('',#1296,.T.);
#903=FACE_OUTER_BOUND('',#1298,.T.);
#904=FACE_OUTER_BOUND('',#1299,.T.);
#905=FACE_OUTER_BOUND('',#1300,.T.);
#906=FACE_OUTER_BOUND('',#1302,.T.);
#907=FACE_OUTER_BOUND('',#1303,.T.);
#908=FACE_OUTER_BOUND('',#1304,.T.);
#909=FACE_OUTER_BOUND('',#1306,.T.);
#910=FACE_OUTER_BOUND('',#1307,.T.);
#911=FACE_OUTER_BOUND('',#1309,.T.);
#912=FACE_OUTER_BOUND('',#1310,.T.);
#913=FACE_OUTER_BOUND('',#1311,.T.);
#914=FACE_OUTER_BOUND('',#1312,.T.);
#915=FACE_OUTER_BOUND('',#1313,.T.);
#916=FACE_OUTER_BOUND('',#1315,.T.);
#917=FACE_OUTER_BOUND('',#1316,.T.);
#918=FACE_OUTER_BOUND('',#1317,.T.);
#919=FACE_OUTER_BOUND('',#1318,.T.);
#920=FACE_OUTER_BOUND('',#1319,.T.);
#921=FACE_OUTER_BOUND('',#1320,.T.);
#922=FACE_OUTER_BOUND('',#1321,.T.);
#923=FACE_OUTER_BOUND('',#1322,.T.);
#924=FACE_OUTER_BOUND('',#1323,.T.);
#925=FACE_OUTER_BOUND('',#1324,.T.);
#926=FACE_OUTER_BOUND('',#1325,.T.);
#927=FACE_OUTER_BOUND('',#1326,.T.);
#928=FACE_OUTER_BOUND('',#1327,.T.);
#929=FACE_OUTER_BOUND('',#1328,.T.);
#930=FACE_OUTER_BOUND('',#1329,.T.);
#931=FACE_OUTER_BOUND('',#1330,.T.);
#932=FACE_OUTER_BOUND('',#1331,.T.);
#933=FACE_OUTER_BOUND('',#1332,.T.);
#934=FACE_OUTER_BOUND('',#1333,.T.);
#935=FACE_OUTER_BOUND('',#1334,.T.);
#936=FACE_OUTER_BOUND('',#1335,.T.);
#937=FACE_OUTER_BOUND('',#1336,.T.);
#938=FACE_OUTER_BOUND('',#1338,.T.);
#939=FACE_OUTER_BOUND('',#1340,.T.);
#940=FACE_OUTER_BOUND('',#1341,.T.);
#941=FACE_OUTER_BOUND('',#1342,.T.);
#942=FACE_OUTER_BOUND('',#1343,.T.);
#943=FACE_OUTER_BOUND('',#1344,.T.);
#944=FACE_OUTER_BOUND('',#1346,.T.);
#945=FACE_OUTER_BOUND('',#1347,.T.);
#946=FACE_OUTER_BOUND('',#1348,.T.);
#947=FACE_OUTER_BOUND('',#1349,.T.);
#948=FACE_OUTER_BOUND('',#1350,.T.);
#949=FACE_OUTER_BOUND('',#1351,.T.);
#950=FACE_OUTER_BOUND('',#1352,.T.);
#951=FACE_OUTER_BOUND('',#1353,.T.);
#952=FACE_OUTER_BOUND('',#1354,.T.);
#953=FACE_OUTER_BOUND('',#1355,.T.);
#954=FACE_OUTER_BOUND('',#1356,.T.);
#955=FACE_OUTER_BOUND('',#1357,.T.);
#956=FACE_OUTER_BOUND('',#1358,.T.);
#957=FACE_OUTER_BOUND('',#1359,.T.);
#958=FACE_OUTER_BOUND('',#1360,.T.);
#959=FACE_OUTER_BOUND('',#1361,.T.);
#960=FACE_OUTER_BOUND('',#1362,.T.);
#961=FACE_OUTER_BOUND('',#1363,.T.);
#962=FACE_OUTER_BOUND('',#1364,.T.);
#963=FACE_OUTER_BOUND('',#1365,.T.);
#964=FACE_OUTER_BOUND('',#1366,.T.);
#965=FACE_OUTER_BOUND('',#1367,.T.);
#966=FACE_OUTER_BOUND('',#1368,.T.);
#967=FACE_OUTER_BOUND('',#1369,.T.);
#968=FACE_OUTER_BOUND('',#1370,.T.);
#969=FACE_OUTER_BOUND('',#1381,.T.);
#970=FACE_OUTER_BOUND('',#1382,.T.);
#971=FACE_OUTER_BOUND('',#1383,.T.);
#972=FACE_OUTER_BOUND('',#1394,.T.);
#973=FACE_OUTER_BOUND('',#1395,.T.);
#974=FACE_OUTER_BOUND('',#1396,.T.);
#975=FACE_OUTER_BOUND('',#1397,.T.);
#976=FACE_OUTER_BOUND('',#1398,.T.);
#977=FACE_OUTER_BOUND('',#1399,.T.);
#978=FACE_OUTER_BOUND('',#1401,.T.);
#979=FACE_OUTER_BOUND('',#1402,.T.);
#980=FACE_OUTER_BOUND('',#1403,.T.);
#981=FACE_OUTER_BOUND('',#1409,.T.);
#982=FACE_OUTER_BOUND('',#1415,.T.);
#983=FACE_OUTER_BOUND('',#1416,.T.);
#984=FACE_OUTER_BOUND('',#1417,.T.);
#985=FACE_OUTER_BOUND('',#1418,.T.);
#986=FACE_OUTER_BOUND('',#1419,.T.);
#987=FACE_OUTER_BOUND('',#1420,.T.);
#988=FACE_OUTER_BOUND('',#1422,.T.);
#989=FACE_OUTER_BOUND('',#1423,.T.);
#990=FACE_OUTER_BOUND('',#1424,.T.);
#991=FACE_OUTER_BOUND('',#1430,.T.);
#992=FACE_OUTER_BOUND('',#1436,.T.);
#993=FACE_OUTER_BOUND('',#1437,.T.);
#994=FACE_OUTER_BOUND('',#1438,.T.);
#995=FACE_OUTER_BOUND('',#1439,.T.);
#996=FACE_OUTER_BOUND('',#1440,.T.);
#997=FACE_OUTER_BOUND('',#1441,.T.);
#998=FACE_OUTER_BOUND('',#1443,.T.);
#999=FACE_OUTER_BOUND('',#1444,.T.);
#1000=FACE_OUTER_BOUND('',#1445,.T.);
#1001=FACE_OUTER_BOUND('',#1451,.T.);
#1002=FACE_OUTER_BOUND('',#1457,.T.);
#1003=FACE_OUTER_BOUND('',#1458,.T.);
#1004=FACE_OUTER_BOUND('',#1459,.T.);
#1005=FACE_OUTER_BOUND('',#1460,.T.);
#1006=FACE_OUTER_BOUND('',#1461,.T.);
#1007=FACE_OUTER_BOUND('',#1462,.T.);
#1008=FACE_OUTER_BOUND('',#1464,.T.);
#1009=FACE_OUTER_BOUND('',#1465,.T.);
#1010=FACE_OUTER_BOUND('',#1466,.T.);
#1011=FACE_OUTER_BOUND('',#1472,.T.);
#1012=FACE_OUTER_BOUND('',#1478,.T.);
#1013=FACE_OUTER_BOUND('',#1479,.T.);
#1014=FACE_OUTER_BOUND('',#1481,.T.);
#1015=FACE_OUTER_BOUND('',#1482,.T.);
#1016=FACE_OUTER_BOUND('',#1483,.T.);
#1017=FACE_OUTER_BOUND('',#1484,.T.);
#1018=FACE_OUTER_BOUND('',#1485,.T.);
#1019=FACE_OUTER_BOUND('',#1486,.T.);
#1020=FACE_OUTER_BOUND('',#1487,.T.);
#1021=FACE_OUTER_BOUND('',#1488,.T.);
#1022=FACE_OUTER_BOUND('',#1489,.T.);
#1023=FACE_OUTER_BOUND('',#1490,.T.);
#1024=FACE_OUTER_BOUND('',#1491,.T.);
#1025=FACE_OUTER_BOUND('',#1492,.T.);
#1026=FACE_OUTER_BOUND('',#1493,.T.);
#1027=FACE_OUTER_BOUND('',#1494,.T.);
#1028=FACE_OUTER_BOUND('',#1496,.T.);
#1029=FACE_OUTER_BOUND('',#1497,.T.);
#1030=FACE_OUTER_BOUND('',#1499,.T.);
#1031=FACE_OUTER_BOUND('',#1500,.T.);
#1032=FACE_OUTER_BOUND('',#1501,.T.);
#1033=FACE_OUTER_BOUND('',#1502,.T.);
#1034=FACE_OUTER_BOUND('',#1504,.T.);
#1035=FACE_OUTER_BOUND('',#1505,.T.);
#1036=FACE_OUTER_BOUND('',#1506,.T.);
#1037=FACE_OUTER_BOUND('',#1507,.T.);
#1038=FACE_OUTER_BOUND('',#1509,.T.);
#1039=FACE_OUTER_BOUND('',#1510,.T.);
#1040=FACE_OUTER_BOUND('',#1511,.T.);
#1041=FACE_OUTER_BOUND('',#1512,.T.);
#1042=FACE_OUTER_BOUND('',#1513,.T.);
#1043=FACE_OUTER_BOUND('',#1514,.T.);
#1044=FACE_OUTER_BOUND('',#1515,.T.);
#1045=FACE_OUTER_BOUND('',#1516,.T.);
#1046=FACE_OUTER_BOUND('',#1517,.T.);
#1047=FACE_OUTER_BOUND('',#1518,.T.);
#1048=FACE_OUTER_BOUND('',#1519,.T.);
#1049=FACE_OUTER_BOUND('',#1520,.T.);
#1050=FACE_OUTER_BOUND('',#1521,.T.);
#1051=FACE_OUTER_BOUND('',#1522,.T.);
#1052=FACE_OUTER_BOUND('',#1523,.T.);
#1053=FACE_OUTER_BOUND('',#1524,.T.);
#1054=FACE_OUTER_BOUND('',#1525,.T.);
#1055=FACE_OUTER_BOUND('',#1526,.T.);
#1056=FACE_OUTER_BOUND('',#1527,.T.);
#1057=FACE_OUTER_BOUND('',#1528,.T.);
#1058=FACE_OUTER_BOUND('',#1529,.T.);
#1059=FACE_OUTER_BOUND('',#1530,.T.);
#1060=FACE_OUTER_BOUND('',#1531,.T.);
#1061=FACE_OUTER_BOUND('',#1532,.T.);
#1062=FACE_OUTER_BOUND('',#1533,.T.);
#1063=FACE_OUTER_BOUND('',#1534,.T.);
#1064=FACE_OUTER_BOUND('',#1535,.T.);
#1065=FACE_OUTER_BOUND('',#1537,.T.);
#1066=FACE_OUTER_BOUND('',#1538,.T.);
#1067=FACE_OUTER_BOUND('',#1540,.T.);
#1068=FACE_OUTER_BOUND('',#1541,.T.);
#1069=FACE_OUTER_BOUND('',#1543,.T.);
#1070=FACE_OUTER_BOUND('',#1544,.T.);
#1071=FACE_OUTER_BOUND('',#1546,.T.);
#1072=FACE_OUTER_BOUND('',#1547,.T.);
#1073=FACE_OUTER_BOUND('',#1549,.T.);
#1074=FACE_OUTER_BOUND('',#1550,.T.);
#1075=FACE_OUTER_BOUND('',#1551,.T.);
#1076=FACE_OUTER_BOUND('',#1552,.T.);
#1077=FACE_OUTER_BOUND('',#1553,.T.);
#1078=FACE_OUTER_BOUND('',#1554,.T.);
#1079=FACE_OUTER_BOUND('',#1555,.T.);
#1080=FACE_OUTER_BOUND('',#1557,.T.);
#1081=FACE_OUTER_BOUND('',#1558,.T.);
#1082=FACE_OUTER_BOUND('',#1559,.T.);
#1083=FACE_OUTER_BOUND('',#1560,.T.);
#1084=FACE_OUTER_BOUND('',#1561,.T.);
#1085=FACE_OUTER_BOUND('',#1562,.T.);
#1086=FACE_OUTER_BOUND('',#1563,.T.);
#1087=FACE_OUTER_BOUND('',#1564,.T.);
#1088=FACE_OUTER_BOUND('',#1565,.T.);
#1089=FACE_OUTER_BOUND('',#1566,.T.);
#1090=FACE_OUTER_BOUND('',#1567,.T.);
#1091=FACE_OUTER_BOUND('',#1568,.T.);
#1092=FACE_OUTER_BOUND('',#1569,.T.);
#1093=FACE_OUTER_BOUND('',#1570,.T.);
#1094=FACE_OUTER_BOUND('',#1572,.T.);
#1095=FACE_OUTER_BOUND('',#1574,.T.);
#1096=FACE_OUTER_BOUND('',#1575,.T.);
#1097=FACE_OUTER_BOUND('',#1576,.T.);
#1098=FACE_OUTER_BOUND('',#1578,.T.);
#1099=FACE_OUTER_BOUND('',#1579,.T.);
#1100=FACE_OUTER_BOUND('',#1580,.T.);
#1101=FACE_OUTER_BOUND('',#1581,.T.);
#1102=FACE_OUTER_BOUND('',#1582,.T.);
#1103=FACE_OUTER_BOUND('',#1584,.T.);
#1104=FACE_OUTER_BOUND('',#1586,.T.);
#1105=FACE_OUTER_BOUND('',#1588,.T.);
#1106=FACE_OUTER_BOUND('',#1590,.T.);
#1107=FACE_OUTER_BOUND('',#1591,.T.);
#1108=FACE_OUTER_BOUND('',#1592,.T.);
#1109=FACE_OUTER_BOUND('',#1594,.T.);
#1110=FACE_OUTER_BOUND('',#1596,.T.);
#1111=FACE_OUTER_BOUND('',#1597,.T.);
#1112=FACE_OUTER_BOUND('',#1598,.T.);
#1113=FACE_OUTER_BOUND('',#1600,.T.);
#1114=FACE_OUTER_BOUND('',#1602,.T.);
#1115=FACE_OUTER_BOUND('',#1603,.T.);
#1116=FACE_OUTER_BOUND('',#1604,.T.);
#1117=FACE_OUTER_BOUND('',#1605,.T.);
#1118=FACE_OUTER_BOUND('',#1606,.T.);
#1119=FACE_OUTER_BOUND('',#1607,.T.);
#1120=FACE_OUTER_BOUND('',#1608,.T.);
#1121=FACE_OUTER_BOUND('',#1609,.T.);
#1122=FACE_OUTER_BOUND('',#1610,.T.);
#1123=FACE_OUTER_BOUND('',#1612,.T.);
#1124=FACE_OUTER_BOUND('',#1614,.T.);
#1125=FACE_OUTER_BOUND('',#1615,.T.);
#1126=FACE_OUTER_BOUND('',#1616,.T.);
#1127=FACE_OUTER_BOUND('',#1617,.T.);
#1128=FACE_OUTER_BOUND('',#1618,.T.);
#1129=FACE_OUTER_BOUND('',#1619,.T.);
#1130=FACE_OUTER_BOUND('',#1620,.T.);
#1131=FACE_OUTER_BOUND('',#1621,.T.);
#1132=FACE_OUTER_BOUND('',#1622,.T.);
#1133=FACE_OUTER_BOUND('',#1624,.T.);
#1134=FACE_OUTER_BOUND('',#1625,.T.);
#1135=FACE_OUTER_BOUND('',#1626,.T.);
#1136=FACE_OUTER_BOUND('',#1627,.T.);
#1137=FACE_OUTER_BOUND('',#1628,.T.);
#1138=FACE_OUTER_BOUND('',#1632,.T.);
#1139=FACE_OUTER_BOUND('',#1633,.T.);
#1140=FACE_OUTER_BOUND('',#1634,.T.);
#1141=FACE_OUTER_BOUND('',#1638,.T.);
#1142=FACE_OUTER_BOUND('',#1640,.T.);
#1143=FACE_OUTER_BOUND('',#1642,.T.);
#1144=FACE_OUTER_BOUND('',#1643,.T.);
#1145=FACE_OUTER_BOUND('',#1645,.T.);
#1146=FACE_OUTER_BOUND('',#1647,.T.);
#1147=FACE_OUTER_BOUND('',#1648,.T.);
#1148=FACE_OUTER_BOUND('',#1650,.T.);
#1149=FACE_OUTER_BOUND('',#1651,.T.);
#1150=FACE_OUTER_BOUND('',#1652,.T.);
#1151=FACE_OUTER_BOUND('',#1653,.T.);
#1152=FACE_OUTER_BOUND('',#1654,.T.);
#1153=FACE_OUTER_BOUND('',#1655,.T.);
#1154=FACE_OUTER_BOUND('',#1656,.T.);
#1155=FACE_OUTER_BOUND('',#1657,.T.);
#1156=FACE_OUTER_BOUND('',#1658,.T.);
#1157=FACE_OUTER_BOUND('',#1659,.T.);
#1158=FACE_OUTER_BOUND('',#1660,.T.);
#1159=FACE_OUTER_BOUND('',#1661,.T.);
#1160=FACE_OUTER_BOUND('',#1662,.T.);
#1161=FACE_OUTER_BOUND('',#1663,.T.);
#1162=FACE_OUTER_BOUND('',#1664,.T.);
#1163=FACE_OUTER_BOUND('',#1665,.T.);
#1164=FACE_OUTER_BOUND('',#1666,.T.);
#1165=FACE_OUTER_BOUND('',#1667,.T.);
#1166=FACE_OUTER_BOUND('',#1668,.T.);
#1167=FACE_OUTER_BOUND('',#1669,.T.);
#1168=FACE_OUTER_BOUND('',#1670,.T.);
#1169=FACE_OUTER_BOUND('',#1671,.T.);
#1170=FACE_OUTER_BOUND('',#1672,.T.);
#1171=FACE_OUTER_BOUND('',#1673,.T.);
#1172=FACE_OUTER_BOUND('',#1674,.T.);
#1173=FACE_OUTER_BOUND('',#1675,.T.);
#1174=FACE_OUTER_BOUND('',#1676,.T.);
#1175=FACE_OUTER_BOUND('',#1677,.T.);
#1176=FACE_OUTER_BOUND('',#1678,.T.);
#1177=FACE_OUTER_BOUND('',#1679,.T.);
#1178=FACE_OUTER_BOUND('',#1680,.T.);
#1179=FACE_OUTER_BOUND('',#1681,.T.);
#1180=FACE_OUTER_BOUND('',#1682,.T.);
#1181=FACE_OUTER_BOUND('',#1683,.T.);
#1182=FACE_OUTER_BOUND('',#1684,.T.);
#1183=FACE_OUTER_BOUND('',#1685,.T.);
#1184=FACE_OUTER_BOUND('',#1686,.T.);
#1185=FACE_OUTER_BOUND('',#1687,.T.);
#1186=FACE_OUTER_BOUND('',#1688,.T.);
#1187=FACE_OUTER_BOUND('',#1689,.T.);
#1188=FACE_OUTER_BOUND('',#1690,.T.);
#1189=FACE_OUTER_BOUND('',#1691,.T.);
#1190=FACE_OUTER_BOUND('',#1692,.T.);
#1191=FACE_OUTER_BOUND('',#1693,.T.);
#1192=FACE_OUTER_BOUND('',#1694,.T.);
#1193=FACE_OUTER_BOUND('',#1695,.T.);
#1194=FACE_OUTER_BOUND('',#1696,.T.);
#1195=FACE_OUTER_BOUND('',#1697,.T.);
#1196=FACE_OUTER_BOUND('',#1698,.T.);
#1197=FACE_OUTER_BOUND('',#1699,.T.);
#1198=FACE_OUTER_BOUND('',#1700,.T.);
#1199=FACE_OUTER_BOUND('',#1701,.T.);
#1200=FACE_OUTER_BOUND('',#1702,.T.);
#1201=FACE_OUTER_BOUND('',#1703,.T.);
#1202=FACE_OUTER_BOUND('',#1705,.T.);
#1203=FACE_OUTER_BOUND('',#1706,.T.);
#1204=EDGE_LOOP('',(#4086,#4087,#4088,#4089));
#1205=EDGE_LOOP('',(#4090,#4091,#4092,#4093));
#1206=EDGE_LOOP('',(#4094,#4095,#4096,#4097));
#1207=EDGE_LOOP('',(#4098,#4099,#4100,#4101));
#1208=EDGE_LOOP('',(#4102,#4103,#4104,#4105));
#1209=EDGE_LOOP('',(#4106,#4107,#4108,#4109));
#1210=EDGE_LOOP('',(#4110,#4111,#4112,#4113));
#1211=EDGE_LOOP('',(#4114,#4115,#4116,#4117));
#1212=EDGE_LOOP('',(#4118,#4119,#4120,#4121));
#1213=EDGE_LOOP('',(#4122,#4123,#4124,#4125));
#1214=EDGE_LOOP('',(#4126));
#1215=EDGE_LOOP('',(#4127));
#1216=EDGE_LOOP('',(#4128));
#1217=EDGE_LOOP('',(#4129));
#1218=EDGE_LOOP('',(#4130));
#1219=EDGE_LOOP('',(#4131,#4132,#4133,#4134));
#1220=EDGE_LOOP('',(#4135));
#1221=EDGE_LOOP('',(#4136));
#1222=EDGE_LOOP('',(#4137));
#1223=EDGE_LOOP('',(#4138));
#1224=EDGE_LOOP('',(#4139));
#1225=EDGE_LOOP('',(#4140,#4141,#4142,#4143));
#1226=EDGE_LOOP('',(#4144,#4145,#4146,#4147));
#1227=EDGE_LOOP('',(#4148,#4149,#4150,#4151));
#1228=EDGE_LOOP('',(#4152,#4153,#4154,#4155));
#1229=EDGE_LOOP('',(#4156,#4157,#4158,#4159));
#1230=EDGE_LOOP('',(#4160,#4161,#4162,#4163));
#1231=EDGE_LOOP('',(#4164,#4165,#4166,#4167));
#1232=EDGE_LOOP('',(#4168,#4169,#4170,#4171));
#1233=EDGE_LOOP('',(#4172,#4173,#4174,#4175));
#1234=EDGE_LOOP('',(#4176,#4177,#4178,#4179));
#1235=EDGE_LOOP('',(#4180,#4181,#4182,#4183));
#1236=EDGE_LOOP('',(#4184,#4185,#4186,#4187));
#1237=EDGE_LOOP('',(#4188,#4189,#4190,#4191));
#1238=EDGE_LOOP('',(#4192,#4193,#4194,#4195));
#1239=EDGE_LOOP('',(#4196,#4197,#4198,#4199));
#1240=EDGE_LOOP('',(#4200));
#1241=EDGE_LOOP('',(#4201));
#1242=EDGE_LOOP('',(#4202,#4203,#4204,#4205));
#1243=EDGE_LOOP('',(#4206,#4207,#4208,#4209));
#1244=EDGE_LOOP('',(#4210));
#1245=EDGE_LOOP('',(#4211));
#1246=EDGE_LOOP('',(#4212));
#1247=EDGE_LOOP('',(#4213));
#1248=EDGE_LOOP('',(#4214));
#1249=EDGE_LOOP('',(#4215));
#1250=EDGE_LOOP('',(#4216,#4217,#4218,#4219));
#1251=EDGE_LOOP('',(#4220,#4221,#4222,#4223));
#1252=EDGE_LOOP('',(#4224));
#1253=EDGE_LOOP('',(#4225));
#1254=EDGE_LOOP('',(#4226));
#1255=EDGE_LOOP('',(#4227));
#1256=EDGE_LOOP('',(#4228));
#1257=EDGE_LOOP('',(#4229));
#1258=EDGE_LOOP('',(#4230,#4231));
#1259=EDGE_LOOP('',(#4232,#4233,#4234,#4235,#4236,#4237,#4238,#4239,#4240));
#1260=EDGE_LOOP('',(#4241,#4242));
#1261=EDGE_LOOP('',(#4243,#4244,#4245,#4246));
#1262=EDGE_LOOP('',(#4247,#4248,#4249,#4250,#4251));
#1263=EDGE_LOOP('',(#4252,#4253,#4254,#4255));
#1264=EDGE_LOOP('',(#4256,#4257));
#1265=EDGE_LOOP('',(#4258));
#1266=EDGE_LOOP('',(#4259));
#1267=EDGE_LOOP('',(#4260));
#1268=EDGE_LOOP('',(#4261));
#1269=EDGE_LOOP('',(#4262,#4263,#4264,#4265));
#1270=EDGE_LOOP('',(#4266));
#1271=EDGE_LOOP('',(#4267,#4268,#4269,#4270));
#1272=EDGE_LOOP('',(#4271,#4272,#4273,#4274));
#1273=EDGE_LOOP('',(#4275));
#1274=EDGE_LOOP('',(#4276));
#1275=EDGE_LOOP('',(#4277));
#1276=EDGE_LOOP('',(#4278));
#1277=EDGE_LOOP('',(#4279));
#1278=EDGE_LOOP('',(#4280,#4281,#4282,#4283,#4284));
#1279=EDGE_LOOP('',(#4285));
#1280=EDGE_LOOP('',(#4286,#4287));
#1281=EDGE_LOOP('',(#4288,#4289,#4290));
#1282=EDGE_LOOP('',(#4291,#4292,#4293,#4294,#4295,#4296,#4297,#4298));
#1283=EDGE_LOOP('',(#4299,#4300));
#1284=EDGE_LOOP('',(#4301,#4302));
#1285=EDGE_LOOP('',(#4303,#4304,#4305,#4306,#4307,#4308,#4309,#4310,#4311,
#4312));
#1286=EDGE_LOOP('',(#4313,#4314,#4315,#4316,#4317));
#1287=EDGE_LOOP('',(#4318,#4319));
#1288=EDGE_LOOP('',(#4320));
#1289=EDGE_LOOP('',(#4321,#4322,#4323));
#1290=EDGE_LOOP('',(#4324,#4325,#4326,#4327));
#1291=EDGE_LOOP('',(#4328));
#1292=EDGE_LOOP('',(#4329,#4330,#4331,#4332));
#1293=EDGE_LOOP('',(#4333,#4334,#4335,#4336));
#1294=EDGE_LOOP('',(#4337));
#1295=EDGE_LOOP('',(#4338,#4339,#4340,#4341));
#1296=EDGE_LOOP('',(#4342,#4343,#4344,#4345));
#1297=EDGE_LOOP('',(#4346));
#1298=EDGE_LOOP('',(#4347,#4348,#4349,#4350));
#1299=EDGE_LOOP('',(#4351,#4352,#4353,#4354));
#1300=EDGE_LOOP('',(#4355,#4356,#4357,#4358));
#1301=EDGE_LOOP('',(#4359));
#1302=EDGE_LOOP('',(#4360,#4361,#4362,#4363));
#1303=EDGE_LOOP('',(#4364,#4365,#4366,#4367));
#1304=EDGE_LOOP('',(#4368));
#1305=EDGE_LOOP('',(#4369));
#1306=EDGE_LOOP('',(#4370,#4371,#4372,#4373));
#1307=EDGE_LOOP('',(#4374));
#1308=EDGE_LOOP('',(#4375));
#1309=EDGE_LOOP('',(#4376));
#1310=EDGE_LOOP('',(#4377,#4378,#4379,#4380));
#1311=EDGE_LOOP('',(#4381,#4382,#4383,#4384));
#1312=EDGE_LOOP('',(#4385,#4386,#4387,#4388));
#1313=EDGE_LOOP('',(#4389));
#1314=EDGE_LOOP('',(#4390));
#1315=EDGE_LOOP('',(#4391,#4392,#4393,#4394));
#1316=EDGE_LOOP('',(#4395,#4396,#4397,#4398));
#1317=EDGE_LOOP('',(#4399,#4400,#4401,#4402));
#1318=EDGE_LOOP('',(#4403));
#1319=EDGE_LOOP('',(#4404,#4405,#4406,#4407));
#1320=EDGE_LOOP('',(#4408,#4409,#4410,#4411));
#1321=EDGE_LOOP('',(#4412,#4413,#4414,#4415));
#1322=EDGE_LOOP('',(#4416,#4417,#4418,#4419));
#1323=EDGE_LOOP('',(#4420,#4421,#4422,#4423));
#1324=EDGE_LOOP('',(#4424,#4425,#4426,#4427));
#1325=EDGE_LOOP('',(#4428,#4429,#4430,#4431,#4432,#4433));
#1326=EDGE_LOOP('',(#4434,#4435,#4436,#4437,#4438,#4439));
#1327=EDGE_LOOP('',(#4440,#4441,#4442,#4443,#4444,#4445,#4446,#4447,#4448));
#1328=EDGE_LOOP('',(#4449,#4450,#4451,#4452,#4453,#4454,#4455,#4456,#4457));
#1329=EDGE_LOOP('',(#4458,#4459,#4460,#4461));
#1330=EDGE_LOOP('',(#4462,#4463,#4464,#4465));
#1331=EDGE_LOOP('',(#4466,#4467,#4468,#4469));
#1332=EDGE_LOOP('',(#4470,#4471,#4472,#4473));
#1333=EDGE_LOOP('',(#4474,#4475,#4476,#4477));
#1334=EDGE_LOOP('',(#4478,#4479,#4480,#4481));
#1335=EDGE_LOOP('',(#4482,#4483,#4484,#4485));
#1336=EDGE_LOOP('',(#4486));
#1337=EDGE_LOOP('',(#4487));
#1338=EDGE_LOOP('',(#4488));
#1339=EDGE_LOOP('',(#4489));
#1340=EDGE_LOOP('',(#4490));
#1341=EDGE_LOOP('',(#4491,#4492,#4493,#4494));
#1342=EDGE_LOOP('',(#4495,#4496,#4497,#4498));
#1343=EDGE_LOOP('',(#4499,#4500,#4501,#4502));
#1344=EDGE_LOOP('',(#4503));
#1345=EDGE_LOOP('',(#4504));
#1346=EDGE_LOOP('',(#4505,#4506,#4507,#4508));
#1347=EDGE_LOOP('',(#4509,#4510,#4511,#4512));
#1348=EDGE_LOOP('',(#4513,#4514,#4515,#4516));
#1349=EDGE_LOOP('',(#4517));
#1350=EDGE_LOOP('',(#4518,#4519,#4520,#4521));
#1351=EDGE_LOOP('',(#4522,#4523,#4524,#4525));
#1352=EDGE_LOOP('',(#4526,#4527,#4528,#4529));
#1353=EDGE_LOOP('',(#4530,#4531,#4532,#4533));
#1354=EDGE_LOOP('',(#4534,#4535,#4536,#4537));
#1355=EDGE_LOOP('',(#4538,#4539,#4540,#4541));
#1356=EDGE_LOOP('',(#4542,#4543,#4544,#4545,#4546,#4547));
#1357=EDGE_LOOP('',(#4548,#4549,#4550,#4551,#4552,#4553));
#1358=EDGE_LOOP('',(#4554,#4555,#4556,#4557));
#1359=EDGE_LOOP('',(#4558,#4559,#4560,#4561));
#1360=EDGE_LOOP('',(#4562,#4563,#4564,#4565));
#1361=EDGE_LOOP('',(#4566,#4567,#4568,#4569));
#1362=EDGE_LOOP('',(#4570,#4571,#4572,#4573));
#1363=EDGE_LOOP('',(#4574,#4575,#4576,#4577));
#1364=EDGE_LOOP('',(#4578,#4579,#4580,#4581));
#1365=EDGE_LOOP('',(#4582,#4583,#4584,#4585));
#1366=EDGE_LOOP('',(#4586,#4587,#4588,#4589));
#1367=EDGE_LOOP('',(#4590,#4591,#4592,#4593));
#1368=EDGE_LOOP('',(#4594,#4595,#4596,#4597));
#1369=EDGE_LOOP('',(#4598,#4599,#4600,#4601));
#1370=EDGE_LOOP('',(#4602,#4603,#4604,#4605));
#1371=EDGE_LOOP('',(#4606));
#1372=EDGE_LOOP('',(#4607));
#1373=EDGE_LOOP('',(#4608));
#1374=EDGE_LOOP('',(#4609));
#1375=EDGE_LOOP('',(#4610));
#1376=EDGE_LOOP('',(#4611));
#1377=EDGE_LOOP('',(#4612));
#1378=EDGE_LOOP('',(#4613));
#1379=EDGE_LOOP('',(#4614));
#1380=EDGE_LOOP('',(#4615));
#1381=EDGE_LOOP('',(#4616,#4617,#4618,#4619));
#1382=EDGE_LOOP('',(#4620,#4621,#4622,#4623));
#1383=EDGE_LOOP('',(#4624,#4625,#4626,#4627));
#1384=EDGE_LOOP('',(#4628));
#1385=EDGE_LOOP('',(#4629));
#1386=EDGE_LOOP('',(#4630));
#1387=EDGE_LOOP('',(#4631));
#1388=EDGE_LOOP('',(#4632));
#1389=EDGE_LOOP('',(#4633));
#1390=EDGE_LOOP('',(#4634));
#1391=EDGE_LOOP('',(#4635));
#1392=EDGE_LOOP('',(#4636));
#1393=EDGE_LOOP('',(#4637));
#1394=EDGE_LOOP('',(#4638,#4639,#4640,#4641));
#1395=EDGE_LOOP('',(#4642,#4643,#4644,#4645));
#1396=EDGE_LOOP('',(#4646,#4647,#4648,#4649));
#1397=EDGE_LOOP('',(#4650,#4651,#4652,#4653));
#1398=EDGE_LOOP('',(#4654,#4655,#4656,#4657));
#1399=EDGE_LOOP('',(#4658));
#1400=EDGE_LOOP('',(#4659));
#1401=EDGE_LOOP('',(#4660,#4661,#4662,#4663));
#1402=EDGE_LOOP('',(#4664,#4665,#4666,#4667));
#1403=EDGE_LOOP('',(#4668));
#1404=EDGE_LOOP('',(#4669));
#1405=EDGE_LOOP('',(#4670));
#1406=EDGE_LOOP('',(#4671));
#1407=EDGE_LOOP('',(#4672));
#1408=EDGE_LOOP('',(#4673));
#1409=EDGE_LOOP('',(#4674));
#1410=EDGE_LOOP('',(#4675));
#1411=EDGE_LOOP('',(#4676));
#1412=EDGE_LOOP('',(#4677));
#1413=EDGE_LOOP('',(#4678));
#1414=EDGE_LOOP('',(#4679));
#1415=EDGE_LOOP('',(#4680,#4681,#4682,#4683));
#1416=EDGE_LOOP('',(#4684,#4685,#4686,#4687));
#1417=EDGE_LOOP('',(#4688,#4689,#4690,#4691));
#1418=EDGE_LOOP('',(#4692,#4693,#4694,#4695));
#1419=EDGE_LOOP('',(#4696,#4697,#4698,#4699));
#1420=EDGE_LOOP('',(#4700));
#1421=EDGE_LOOP('',(#4701));
#1422=EDGE_LOOP('',(#4702,#4703,#4704,#4705));
#1423=EDGE_LOOP('',(#4706,#4707,#4708,#4709));
#1424=EDGE_LOOP('',(#4710));
#1425=EDGE_LOOP('',(#4711));
#1426=EDGE_LOOP('',(#4712));
#1427=EDGE_LOOP('',(#4713));
#1428=EDGE_LOOP('',(#4714));
#1429=EDGE_LOOP('',(#4715));
#1430=EDGE_LOOP('',(#4716));
#1431=EDGE_LOOP('',(#4717));
#1432=EDGE_LOOP('',(#4718));
#1433=EDGE_LOOP('',(#4719));
#1434=EDGE_LOOP('',(#4720));
#1435=EDGE_LOOP('',(#4721));
#1436=EDGE_LOOP('',(#4722,#4723,#4724,#4725));
#1437=EDGE_LOOP('',(#4726,#4727,#4728,#4729));
#1438=EDGE_LOOP('',(#4730,#4731,#4732,#4733));
#1439=EDGE_LOOP('',(#4734,#4735,#4736,#4737));
#1440=EDGE_LOOP('',(#4738,#4739,#4740,#4741));
#1441=EDGE_LOOP('',(#4742));
#1442=EDGE_LOOP('',(#4743));
#1443=EDGE_LOOP('',(#4744,#4745,#4746,#4747));
#1444=EDGE_LOOP('',(#4748,#4749,#4750,#4751));
#1445=EDGE_LOOP('',(#4752));
#1446=EDGE_LOOP('',(#4753));
#1447=EDGE_LOOP('',(#4754));
#1448=EDGE_LOOP('',(#4755));
#1449=EDGE_LOOP('',(#4756));
#1450=EDGE_LOOP('',(#4757));
#1451=EDGE_LOOP('',(#4758));
#1452=EDGE_LOOP('',(#4759));
#1453=EDGE_LOOP('',(#4760));
#1454=EDGE_LOOP('',(#4761));
#1455=EDGE_LOOP('',(#4762));
#1456=EDGE_LOOP('',(#4763));
#1457=EDGE_LOOP('',(#4764,#4765,#4766,#4767));
#1458=EDGE_LOOP('',(#4768,#4769,#4770,#4771));
#1459=EDGE_LOOP('',(#4772,#4773,#4774,#4775));
#1460=EDGE_LOOP('',(#4776,#4777,#4778,#4779));
#1461=EDGE_LOOP('',(#4780,#4781,#4782,#4783));
#1462=EDGE_LOOP('',(#4784));
#1463=EDGE_LOOP('',(#4785));
#1464=EDGE_LOOP('',(#4786,#4787,#4788,#4789));
#1465=EDGE_LOOP('',(#4790,#4791,#4792,#4793));
#1466=EDGE_LOOP('',(#4794));
#1467=EDGE_LOOP('',(#4795));
#1468=EDGE_LOOP('',(#4796));
#1469=EDGE_LOOP('',(#4797));
#1470=EDGE_LOOP('',(#4798));
#1471=EDGE_LOOP('',(#4799));
#1472=EDGE_LOOP('',(#4800));
#1473=EDGE_LOOP('',(#4801));
#1474=EDGE_LOOP('',(#4802));
#1475=EDGE_LOOP('',(#4803));
#1476=EDGE_LOOP('',(#4804));
#1477=EDGE_LOOP('',(#4805));
#1478=EDGE_LOOP('',(#4806,#4807,#4808,#4809,#4810,#4811,#4812));
#1479=EDGE_LOOP('',(#4813,#4814,#4815,#4816,#4817,#4818,#4819,#4820,#4821,
#4822,#4823));
#1480=EDGE_LOOP('',(#4824,#4825));
#1481=EDGE_LOOP('',(#4826));
#1482=EDGE_LOOP('',(#4827,#4828,#4829));
#1483=EDGE_LOOP('',(#4830,#4831,#4832));
#1484=EDGE_LOOP('',(#4833,#4834,#4835,#4836));
#1485=EDGE_LOOP('',(#4837,#4838,#4839,#4840,#4841));
#1486=EDGE_LOOP('',(#4842,#4843,#4844,#4845,#4846));
#1487=EDGE_LOOP('',(#4847,#4848,#4849,#4850));
#1488=EDGE_LOOP('',(#4851,#4852,#4853,#4854,#4855));
#1489=EDGE_LOOP('',(#4856,#4857,#4858,#4859));
#1490=EDGE_LOOP('',(#4860,#4861,#4862,#4863,#4864,#4865));
#1491=EDGE_LOOP('',(#4866,#4867,#4868,#4869,#4870));
#1492=EDGE_LOOP('',(#4871,#4872,#4873,#4874));
#1493=EDGE_LOOP('',(#4875,#4876,#4877,#4878));
#1494=EDGE_LOOP('',(#4879));
#1495=EDGE_LOOP('',(#4880));
#1496=EDGE_LOOP('',(#4881,#4882,#4883,#4884,#4885));
#1497=EDGE_LOOP('',(#4886));
#1498=EDGE_LOOP('',(#4887));
#1499=EDGE_LOOP('',(#4888,#4889,#4890,#4891));
#1500=EDGE_LOOP('',(#4892,#4893,#4894,#4895,#4896,#4897));
#1501=EDGE_LOOP('',(#4898,#4899,#4900,#4901,#4902));
#1502=EDGE_LOOP('',(#4903));
#1503=EDGE_LOOP('',(#4904));
#1504=EDGE_LOOP('',(#4905,#4906,#4907,#4908));
#1505=EDGE_LOOP('',(#4909,#4910,#4911,#4912));
#1506=EDGE_LOOP('',(#4913,#4914,#4915,#4916));
#1507=EDGE_LOOP('',(#4917));
#1508=EDGE_LOOP('',(#4918));
#1509=EDGE_LOOP('',(#4919,#4920,#4921,#4922,#4923));
#1510=EDGE_LOOP('',(#4924,#4925));
#1511=EDGE_LOOP('',(#4926,#4927));
#1512=EDGE_LOOP('',(#4928,#4929));
#1513=EDGE_LOOP('',(#4930,#4931));
#1514=EDGE_LOOP('',(#4932,#4933));
#1515=EDGE_LOOP('',(#4934,#4935));
#1516=EDGE_LOOP('',(#4936,#4937));
#1517=EDGE_LOOP('',(#4938,#4939));
#1518=EDGE_LOOP('',(#4940,#4941,#4942,#4943));
#1519=EDGE_LOOP('',(#4944,#4945,#4946,#4947,#4948,#4949,#4950,#4951,#4952,
#4953,#4954,#4955,#4956,#4957,#4958,#4959,#4960,#4961,#4962,#4963));
#1520=EDGE_LOOP('',(#4964,#4965,#4966,#4967));
#1521=EDGE_LOOP('',(#4968,#4969,#4970,#4971));
#1522=EDGE_LOOP('',(#4972,#4973,#4974,#4975));
#1523=EDGE_LOOP('',(#4976,#4977,#4978,#4979));
#1524=EDGE_LOOP('',(#4980,#4981,#4982,#4983));
#1525=EDGE_LOOP('',(#4984,#4985,#4986,#4987,#4988,#4989));
#1526=EDGE_LOOP('',(#4990,#4991,#4992,#4993));
#1527=EDGE_LOOP('',(#4994,#4995,#4996,#4997));
#1528=EDGE_LOOP('',(#4998,#4999,#5000,#5001));
#1529=EDGE_LOOP('',(#5002,#5003,#5004,#5005));
#1530=EDGE_LOOP('',(#5006,#5007,#5008,#5009));
#1531=EDGE_LOOP('',(#5010,#5011,#5012,#5013));
#1532=EDGE_LOOP('',(#5014,#5015,#5016,#5017,#5018,#5019,#5020,#5021,#5022,
#5023,#5024,#5025,#5026,#5027,#5028,#5029,#5030,#5031,#5032,#5033));
#1533=EDGE_LOOP('',(#5034,#5035,#5036,#5037));
#1534=EDGE_LOOP('',(#5038,#5039,#5040,#5041));
#1535=EDGE_LOOP('',(#5042));
#1536=EDGE_LOOP('',(#5043));
#1537=EDGE_LOOP('',(#5044,#5045,#5046,#5047));
#1538=EDGE_LOOP('',(#5048));
#1539=EDGE_LOOP('',(#5049));
#1540=EDGE_LOOP('',(#5050,#5051,#5052,#5053));
#1541=EDGE_LOOP('',(#5054));
#1542=EDGE_LOOP('',(#5055));
#1543=EDGE_LOOP('',(#5056,#5057,#5058,#5059));
#1544=EDGE_LOOP('',(#5060));
#1545=EDGE_LOOP('',(#5061));
#1546=EDGE_LOOP('',(#5062,#5063,#5064,#5065));
#1547=EDGE_LOOP('',(#5066));
#1548=EDGE_LOOP('',(#5067));
#1549=EDGE_LOOP('',(#5068,#5069,#5070,#5071));
#1550=EDGE_LOOP('',(#5072));
#1551=EDGE_LOOP('',(#5073));
#1552=EDGE_LOOP('',(#5074,#5075,#5076,#5077));
#1553=EDGE_LOOP('',(#5078,#5079,#5080,#5081));
#1554=EDGE_LOOP('',(#5082,#5083,#5084,#5085));
#1555=EDGE_LOOP('',(#5086));
#1556=EDGE_LOOP('',(#5087));
#1557=EDGE_LOOP('',(#5088,#5089,#5090,#5091));
#1558=EDGE_LOOP('',(#5092,#5093,#5094,#5095));
#1559=EDGE_LOOP('',(#5096,#5097,#5098,#5099));
#1560=EDGE_LOOP('',(#5100,#5101,#5102,#5103));
#1561=EDGE_LOOP('',(#5104,#5105,#5106,#5107));
#1562=EDGE_LOOP('',(#5108,#5109,#5110,#5111));
#1563=EDGE_LOOP('',(#5112,#5113,#5114,#5115));
#1564=EDGE_LOOP('',(#5116,#5117,#5118,#5119));
#1565=EDGE_LOOP('',(#5120,#5121,#5122,#5123,#5124,#5125));
#1566=EDGE_LOOP('',(#5126,#5127,#5128,#5129,#5130,#5131));
#1567=EDGE_LOOP('',(#5132,#5133,#5134,#5135));
#1568=EDGE_LOOP('',(#5136));
#1569=EDGE_LOOP('',(#5137,#5138,#5139,#5140));
#1570=EDGE_LOOP('',(#5141));
#1571=EDGE_LOOP('',(#5142));
#1572=EDGE_LOOP('',(#5143));
#1573=EDGE_LOOP('',(#5144));
#1574=EDGE_LOOP('',(#5145,#5146,#5147,#5148));
#1575=EDGE_LOOP('',(#5149,#5150,#5151,#5152));
#1576=EDGE_LOOP('',(#5153));
#1577=EDGE_LOOP('',(#5154));
#1578=EDGE_LOOP('',(#5155));
#1579=EDGE_LOOP('',(#5156,#5157));
#1580=EDGE_LOOP('',(#5158,#5159,#5160,#5161,#5162,#5163,#5164,#5165,#5166));
#1581=EDGE_LOOP('',(#5167,#5168));
#1582=EDGE_LOOP('',(#5169,#5170,#5171,#5172));
#1583=EDGE_LOOP('',(#5173,#5174,#5175,#5176,#5177));
#1584=EDGE_LOOP('',(#5178,#5179,#5180,#5181));
#1585=EDGE_LOOP('',(#5182,#5183));
#1586=EDGE_LOOP('',(#5184));
#1587=EDGE_LOOP('',(#5185));
#1588=EDGE_LOOP('',(#5186));
#1589=EDGE_LOOP('',(#5187));
#1590=EDGE_LOOP('',(#5188,#5189,#5190,#5191));
#1591=EDGE_LOOP('',(#5192,#5193,#5194,#5195));
#1592=EDGE_LOOP('',(#5196));
#1593=EDGE_LOOP('',(#5197));
#1594=EDGE_LOOP('',(#5198));
#1595=EDGE_LOOP('',(#5199));
#1596=EDGE_LOOP('',(#5200,#5201,#5202,#5203));
#1597=EDGE_LOOP('',(#5204,#5205,#5206,#5207));
#1598=EDGE_LOOP('',(#5208));
#1599=EDGE_LOOP('',(#5209));
#1600=EDGE_LOOP('',(#5210));
#1601=EDGE_LOOP('',(#5211));
#1602=EDGE_LOOP('',(#5212,#5213,#5214,#5215));
#1603=EDGE_LOOP('',(#5216));
#1604=EDGE_LOOP('',(#5217));
#1605=EDGE_LOOP('',(#5218,#5219,#5220,#5221));
#1606=EDGE_LOOP('',(#5222));
#1607=EDGE_LOOP('',(#5223));
#1608=EDGE_LOOP('',(#5224,#5225,#5226,#5227));
#1609=EDGE_LOOP('',(#5228,#5229,#5230,#5231));
#1610=EDGE_LOOP('',(#5232));
#1611=EDGE_LOOP('',(#5233));
#1612=EDGE_LOOP('',(#5234));
#1613=EDGE_LOOP('',(#5235));
#1614=EDGE_LOOP('',(#5236));
#1615=EDGE_LOOP('',(#5237,#5238,#5239,#5240));
#1616=EDGE_LOOP('',(#5241,#5242,#5243,#5244));
#1617=EDGE_LOOP('',(#5245,#5246,#5247,#5248));
#1618=EDGE_LOOP('',(#5249,#5250,#5251,#5252));
#1619=EDGE_LOOP('',(#5253,#5254,#5255,#5256));
#1620=EDGE_LOOP('',(#5257,#5258,#5259,#5260));
#1621=EDGE_LOOP('',(#5261,#5262,#5263,#5264,#5265,#5266));
#1622=EDGE_LOOP('',(#5267));
#1623=EDGE_LOOP('',(#5268,#5269,#5270,#5271,#5272,#5273));
#1624=EDGE_LOOP('',(#5274,#5275,#5276,#5277));
#1625=EDGE_LOOP('',(#5278,#5279,#5280,#5281));
#1626=EDGE_LOOP('',(#5282,#5283,#5284,#5285,#5286,#5287,#5288,#5289,#5290));
#1627=EDGE_LOOP('',(#5291,#5292,#5293,#5294,#5295,#5296,#5297));
#1628=EDGE_LOOP('',(#5298,#5299,#5300,#5301,#5302,#5303,#5304,#5305,#5306));
#1629=EDGE_LOOP('',(#5307,#5308,#5309));
#1630=EDGE_LOOP('',(#5310,#5311,#5312));
#1631=EDGE_LOOP('',(#5313,#5314,#5315));
#1632=EDGE_LOOP('',(#5316,#5317,#5318,#5319,#5320,#5321,#5322));
#1633=EDGE_LOOP('',(#5323,#5324,#5325,#5326,#5327,#5328,#5329));
#1634=EDGE_LOOP('',(#5330,#5331,#5332,#5333,#5334,#5335,#5336,#5337,#5338,
#5339));
#1635=EDGE_LOOP('',(#5340,#5341));
#1636=EDGE_LOOP('',(#5342,#5343));
#1637=EDGE_LOOP('',(#5344,#5345));
#1638=EDGE_LOOP('',(#5346));
#1639=EDGE_LOOP('',(#5347));
#1640=EDGE_LOOP('',(#5348));
#1641=EDGE_LOOP('',(#5349,#5350,#5351,#5352,#5353,#5354,#5355,#5356,#5357,
#5358,#5359,#5360,#5361,#5362,#5363,#5364,#5365,#5366,#5367,#5368,#5369,
#5370,#5371,#5372,#5373,#5374,#5375,#5376,#5377,#5378,#5379,#5380,#5381,
#5382,#5383,#5384,#5385,#5386,#5387,#5388));
#1642=EDGE_LOOP('',(#5389,#5390,#5391,#5392));
#1643=EDGE_LOOP('',(#5393));
#1644=EDGE_LOOP('',(#5394));
#1645=EDGE_LOOP('',(#5395));
#1646=EDGE_LOOP('',(#5396,#5397,#5398,#5399,#5400,#5401,#5402,#5403,#5404,
#5405,#5406,#5407,#5408,#5409,#5410,#5411,#5412,#5413,#5414,#5415,#5416,
#5417,#5418,#5419,#5420,#5421,#5422,#5423,#5424,#5425,#5426,#5427,#5428,
#5429,#5430,#5431,#5432,#5433,#5434,#5435));
#1647=EDGE_LOOP('',(#5436,#5437,#5438,#5439));
#1648=EDGE_LOOP('',(#5440));
#1649=EDGE_LOOP('',(#5441));
#1650=EDGE_LOOP('',(#5442,#5443,#5444,#5445));
#1651=EDGE_LOOP('',(#5446,#5447,#5448,#5449));
#1652=EDGE_LOOP('',(#5450,#5451,#5452,#5453));
#1653=EDGE_LOOP('',(#5454,#5455,#5456,#5457));
#1654=EDGE_LOOP('',(#5458,#5459,#5460,#5461));
#1655=EDGE_LOOP('',(#5462,#5463,#5464,#5465));
#1656=EDGE_LOOP('',(#5466,#5467,#5468,#5469));
#1657=EDGE_LOOP('',(#5470,#5471,#5472,#5473));
#1658=EDGE_LOOP('',(#5474,#5475,#5476,#5477));
#1659=EDGE_LOOP('',(#5478,#5479,#5480,#5481));
#1660=EDGE_LOOP('',(#5482,#5483,#5484,#5485));
#1661=EDGE_LOOP('',(#5486,#5487,#5488,#5489));
#1662=EDGE_LOOP('',(#5490,#5491,#5492,#5493));
#1663=EDGE_LOOP('',(#5494,#5495,#5496,#5497));
#1664=EDGE_LOOP('',(#5498,#5499,#5500,#5501));
#1665=EDGE_LOOP('',(#5502,#5503,#5504,#5505));
#1666=EDGE_LOOP('',(#5506,#5507,#5508,#5509));
#1667=EDGE_LOOP('',(#5510,#5511,#5512,#5513));
#1668=EDGE_LOOP('',(#5514,#5515,#5516,#5517));
#1669=EDGE_LOOP('',(#5518,#5519,#5520,#5521));
#1670=EDGE_LOOP('',(#5522,#5523,#5524,#5525));
#1671=EDGE_LOOP('',(#5526,#5527,#5528,#5529));
#1672=EDGE_LOOP('',(#5530,#5531,#5532,#5533));
#1673=EDGE_LOOP('',(#5534,#5535,#5536,#5537));
#1674=EDGE_LOOP('',(#5538,#5539,#5540,#5541));
#1675=EDGE_LOOP('',(#5542,#5543,#5544,#5545));
#1676=EDGE_LOOP('',(#5546,#5547,#5548,#5549));
#1677=EDGE_LOOP('',(#5550,#5551,#5552,#5553));
#1678=EDGE_LOOP('',(#5554,#5555,#5556,#5557));
#1679=EDGE_LOOP('',(#5558,#5559,#5560,#5561));
#1680=EDGE_LOOP('',(#5562,#5563,#5564,#5565));
#1681=EDGE_LOOP('',(#5566,#5567,#5568,#5569));
#1682=EDGE_LOOP('',(#5570,#5571,#5572,#5573));
#1683=EDGE_LOOP('',(#5574,#5575,#5576,#5577));
#1684=EDGE_LOOP('',(#5578,#5579,#5580,#5581));
#1685=EDGE_LOOP('',(#5582,#5583,#5584,#5585));
#1686=EDGE_LOOP('',(#5586,#5587,#5588,#5589));
#1687=EDGE_LOOP('',(#5590,#5591,#5592,#5593));
#1688=EDGE_LOOP('',(#5594,#5595,#5596,#5597));
#1689=EDGE_LOOP('',(#5598,#5599,#5600,#5601));
#1690=EDGE_LOOP('',(#5602,#5603,#5604,#5605));
#1691=EDGE_LOOP('',(#5606,#5607,#5608,#5609));
#1692=EDGE_LOOP('',(#5610,#5611,#5612,#5613));
#1693=EDGE_LOOP('',(#5614,#5615,#5616,#5617));
#1694=EDGE_LOOP('',(#5618,#5619,#5620,#5621));
#1695=EDGE_LOOP('',(#5622,#5623,#5624,#5625));
#1696=EDGE_LOOP('',(#5626,#5627,#5628,#5629,#5630,#5631));
#1697=EDGE_LOOP('',(#5632,#5633,#5634,#5635,#5636,#5637));
#1698=EDGE_LOOP('',(#5638));
#1699=EDGE_LOOP('',(#5639));
#1700=EDGE_LOOP('',(#5640,#5641,#5642,#5643));
#1701=EDGE_LOOP('',(#5644,#5645,#5646,#5647));
#1702=EDGE_LOOP('',(#5648,#5649,#5650,#5651));
#1703=EDGE_LOOP('',(#5652));
#1704=EDGE_LOOP('',(#5653));
#1705=EDGE_LOOP('',(#5654,#5655,#5656,#5657));
#1706=EDGE_LOOP('',(#5658,#5659,#5660,#5661));
#1707=LINE('',#9451,#2056);
#1708=LINE('',#9457,#2057);
#1709=LINE('',#9463,#2058);
#1710=LINE('',#9469,#2059);
#1711=LINE('',#9475,#2060);
#1712=LINE('',#9480,#2061);
#1713=LINE('',#9482,#2062);
#1714=LINE('',#9484,#2063);
#1715=LINE('',#9485,#2064);
#1716=LINE('',#9488,#2065);
#1717=LINE('',#9490,#2066);
#1718=LINE('',#9491,#2067);
#1719=LINE('',#9494,#2068);
#1720=LINE('',#9496,#2069);
#1721=LINE('',#9497,#2070);
#1722=LINE('',#9499,#2071);
#1723=LINE('',#9500,#2072);
#1724=LINE('',#9507,#2073);
#1725=LINE('',#9509,#2074);
#1726=LINE('',#9511,#2075);
#1727=LINE('',#9512,#2076);
#1728=LINE('',#9515,#2077);
#1729=LINE('',#9517,#2078);
#1730=LINE('',#9518,#2079);
#1731=LINE('',#9521,#2080);
#1732=LINE('',#9523,#2081);
#1733=LINE('',#9524,#2082);
#1734=LINE('',#9526,#2083);
#1735=LINE('',#9527,#2084);
#1736=LINE('',#9534,#2085);
#1737=LINE('',#9536,#2086);
#1738=LINE('',#9538,#2087);
#1739=LINE('',#9539,#2088);
#1740=LINE('',#9542,#2089);
#1741=LINE('',#9544,#2090);
#1742=LINE('',#9545,#2091);
#1743=LINE('',#9548,#2092);
#1744=LINE('',#9550,#2093);
#1745=LINE('',#9551,#2094);
#1746=LINE('',#9553,#2095);
#1747=LINE('',#9554,#2096);
#1748=LINE('',#9562,#2097);
#1749=LINE('',#9568,#2098);
#1750=LINE('',#9574,#2099);
#1751=LINE('',#9583,#2100);
#1752=LINE('',#9588,#2101);
#1753=LINE('',#9597,#2102);
#1754=LINE('',#9602,#2103);
#1755=LINE('',#9609,#2104);
#1756=LINE('',#9639,#2105);
#1757=LINE('',#9686,#2106);
#1758=LINE('',#9691,#2107);
#1759=LINE('',#9697,#2108);
#1760=LINE('',#9706,#2109);
#1761=LINE('',#9746,#2110);
#1762=LINE('',#9785,#2111);
#1763=LINE('',#9794,#2112);
#1764=LINE('',#9800,#2113);
#1765=LINE('',#9875,#2114);
#1766=LINE('',#9877,#2115);
#1767=LINE('',#10405,#2116);
#1768=LINE('',#10408,#2117);
#1769=LINE('',#10416,#2118);
#1770=LINE('',#10423,#2119);
#1771=LINE('',#10428,#2120);
#1772=LINE('',#10430,#2121);
#1773=LINE('',#10432,#2122);
#1774=LINE('',#10433,#2123);
#1775=LINE('',#10436,#2124);
#1776=LINE('',#10438,#2125);
#1777=LINE('',#10439,#2126);
#1778=LINE('',#10442,#2127);
#1779=LINE('',#10444,#2128);
#1780=LINE('',#10445,#2129);
#1781=LINE('',#10447,#2130);
#1782=LINE('',#10448,#2131);
#1783=LINE('',#10456,#2132);
#1784=LINE('',#10460,#2133);
#1785=LINE('',#10467,#2134);
#1786=LINE('',#10477,#2135);
#1787=LINE('',#10481,#2136);
#1788=LINE('',#10485,#2137);
#1789=LINE('',#10492,#2138);
#1790=LINE('',#10496,#2139);
#1791=LINE('',#10500,#2140);
#1792=LINE('',#10505,#2141);
#1793=LINE('',#10507,#2142);
#1794=LINE('',#10509,#2143);
#1795=LINE('',#10510,#2144);
#1796=LINE('',#10513,#2145);
#1797=LINE('',#10515,#2146);
#1798=LINE('',#10516,#2147);
#1799=LINE('',#10519,#2148);
#1800=LINE('',#10521,#2149);
#1801=LINE('',#10522,#2150);
#1802=LINE('',#10525,#2151);
#1803=LINE('',#10527,#2152);
#1804=LINE('',#10528,#2153);
#1805=LINE('',#10531,#2154);
#1806=LINE('',#10533,#2155);
#1807=LINE('',#10534,#2156);
#1808=LINE('',#10536,#2157);
#1809=LINE('',#10537,#2158);
#1810=LINE('',#10552,#2159);
#1811=LINE('',#10573,#2160);
#1812=LINE('',#10598,#2161);
#1813=LINE('',#10599,#2162);
#1814=LINE('',#10601,#2163);
#1815=LINE('',#10603,#2164);
#1816=LINE('',#10608,#2165);
#1817=LINE('',#10611,#2166);
#1818=LINE('',#10613,#2167);
#1819=LINE('',#10624,#2168);
#1820=LINE('',#10628,#2169);
#1821=LINE('',#10632,#2170);
#1822=LINE('',#10639,#2171);
#1823=LINE('',#10643,#2172);
#1824=LINE('',#10647,#2173);
#1825=LINE('',#10652,#2174);
#1826=LINE('',#10654,#2175);
#1827=LINE('',#10656,#2176);
#1828=LINE('',#10657,#2177);
#1829=LINE('',#10660,#2178);
#1830=LINE('',#10662,#2179);
#1831=LINE('',#10663,#2180);
#1832=LINE('',#10666,#2181);
#1833=LINE('',#10668,#2182);
#1834=LINE('',#10669,#2183);
#1835=LINE('',#10672,#2184);
#1836=LINE('',#10674,#2185);
#1837=LINE('',#10675,#2186);
#1838=LINE('',#10678,#2187);
#1839=LINE('',#10680,#2188);
#1840=LINE('',#10681,#2189);
#1841=LINE('',#10683,#2190);
#1842=LINE('',#10684,#2191);
#1843=LINE('',#10693,#2192);
#1844=LINE('',#10699,#2193);
#1845=LINE('',#10705,#2194);
#1846=LINE('',#10711,#2195);
#1847=LINE('',#10717,#2196);
#1848=LINE('',#10723,#2197);
#1849=LINE('',#10729,#2198);
#1850=LINE('',#10735,#2199);
#1851=LINE('',#10741,#2200);
#1852=LINE('',#10747,#2201);
#1853=LINE('',#10752,#2202);
#1854=LINE('',#10756,#2203);
#1855=LINE('',#10760,#2204);
#1856=LINE('',#10762,#2205);
#1857=LINE('',#10763,#2206);
#1858=LINE('',#10766,#2207);
#1859=LINE('',#10770,#2208);
#1860=LINE('',#10771,#2209);
#1861=LINE('',#10780,#2210);
#1862=LINE('',#10786,#2211);
#1863=LINE('',#10792,#2212);
#1864=LINE('',#10798,#2213);
#1865=LINE('',#10804,#2214);
#1866=LINE('',#10811,#2215);
#1867=LINE('',#10817,#2216);
#1868=LINE('',#10826,#2217);
#1869=LINE('',#10832,#2218);
#1870=LINE('',#10838,#2219);
#1871=LINE('',#10844,#2220);
#1872=LINE('',#10850,#2221);
#1873=LINE('',#10858,#2222);
#1874=LINE('',#10863,#2223);
#1875=LINE('',#10872,#2224);
#1876=LINE('',#10878,#2225);
#1877=LINE('',#10884,#2226);
#1878=LINE('',#10890,#2227);
#1879=LINE('',#10896,#2228);
#1880=LINE('',#10903,#2229);
#1881=LINE('',#10909,#2230);
#1882=LINE('',#10918,#2231);
#1883=LINE('',#10924,#2232);
#1884=LINE('',#10930,#2233);
#1885=LINE('',#10936,#2234);
#1886=LINE('',#10942,#2235);
#1887=LINE('',#10950,#2236);
#1888=LINE('',#10955,#2237);
#1889=LINE('',#11003,#2238);
#1890=LINE('',#11044,#2239);
#1891=LINE('',#11046,#2240);
#1892=LINE('',#11055,#2241);
#1893=LINE('',#11056,#2242);
#1894=LINE('',#11059,#2243);
#1895=LINE('',#11060,#2244);
#1896=LINE('',#11063,#2245);
#1897=LINE('',#11065,#2246);
#1898=LINE('',#11066,#2247);
#1899=LINE('',#11070,#2248);
#1900=LINE('',#11071,#2249);
#1901=LINE('',#11072,#2250);
#1902=LINE('',#11075,#2251);
#1903=LINE('',#11076,#2252);
#1904=LINE('',#11079,#2253);
#1905=LINE('',#11080,#2254);
#1906=LINE('',#11082,#2255);
#1907=LINE('',#11098,#2256);
#1908=LINE('',#11104,#2257);
#1909=LINE('',#11108,#2258);
#1910=LINE('',#11114,#2259);
#1911=LINE('',#11119,#2260);
#1912=LINE('',#11134,#2261);
#1913=LINE('',#11143,#2262);
#1914=LINE('',#11147,#2263);
#1915=LINE('',#11151,#2264);
#1916=LINE('',#11154,#2265);
#1917=LINE('',#11307,#2266);
#1918=LINE('',#11603,#2267);
#1919=LINE('',#11645,#2268);
#1920=LINE('',#11650,#2269);
#1921=LINE('',#11659,#2270);
#1922=LINE('',#11664,#2271);
#1923=LINE('',#11680,#2272);
#1924=LINE('',#11684,#2273);
#1925=LINE('',#11688,#2274);
#1926=LINE('',#11695,#2275);
#1927=LINE('',#11697,#2276);
#1928=LINE('',#11701,#2277);
#1929=LINE('',#11703,#2278);
#1930=LINE('',#11705,#2279);
#1931=LINE('',#11706,#2280);
#1932=LINE('',#11709,#2281);
#1933=LINE('',#11711,#2282);
#1934=LINE('',#11712,#2283);
#1935=LINE('',#11715,#2284);
#1936=LINE('',#11717,#2285);
#1937=LINE('',#11718,#2286);
#1938=LINE('',#11721,#2287);
#1939=LINE('',#11723,#2288);
#1940=LINE('',#11724,#2289);
#1941=LINE('',#11727,#2290);
#1942=LINE('',#11729,#2291);
#1943=LINE('',#11730,#2292);
#1944=LINE('',#11732,#2293);
#1945=LINE('',#11733,#2294);
#1946=LINE('',#11766,#2295);
#1947=LINE('',#11773,#2296);
#1948=LINE('',#11784,#2297);
#1949=LINE('',#11787,#2298);
#1950=LINE('',#11795,#2299);
#1951=LINE('',#11825,#2300);
#1952=LINE('',#11872,#2301);
#1953=LINE('',#11877,#2302);
#1954=LINE('',#11883,#2303);
#1955=LINE('',#11892,#2304);
#1956=LINE('',#11898,#2305);
#1957=LINE('',#11907,#2306);
#1958=LINE('',#11913,#2307);
#1959=LINE('',#11922,#2308);
#1960=LINE('',#11931,#2309);
#1961=LINE('',#11940,#2310);
#1962=LINE('',#11946,#2311);
#1963=LINE('',#11957,#2312);
#1964=LINE('',#11959,#2313);
#1965=LINE('',#11961,#2314);
#1966=LINE('',#11962,#2315);
#1967=LINE('',#11965,#2316);
#1968=LINE('',#11967,#2317);
#1969=LINE('',#11968,#2318);
#1970=LINE('',#11971,#2319);
#1971=LINE('',#11973,#2320);
#1972=LINE('',#11974,#2321);
#1973=LINE('',#11977,#2322);
#1974=LINE('',#11979,#2323);
#1975=LINE('',#11980,#2324);
#1976=LINE('',#11983,#2325);
#1977=LINE('',#11985,#2326);
#1978=LINE('',#11986,#2327);
#1979=LINE('',#11988,#2328);
#1980=LINE('',#11989,#2329);
#1981=LINE('',#11997,#2330);
#1982=LINE('',#11999,#2331);
#1983=LINE('',#12063,#2332);
#1984=LINE('',#12147,#2333);
#1985=LINE('',#12191,#2334);
#1986=LINE('',#12193,#2335);
#1987=LINE('',#12279,#2336);
#1988=LINE('',#12356,#2337);
#1989=LINE('',#12360,#2338);
#1990=LINE('',#12362,#2339);
#1991=LINE('',#12451,#2340);
#1992=LINE('',#12539,#2341);
#1993=LINE('',#12542,#2342);
#1994=LINE('',#12543,#2343);
#1995=LINE('',#12545,#2344);
#1996=LINE('',#12547,#2345);
#1997=LINE('',#12549,#2346);
#1998=LINE('',#12551,#2347);
#1999=LINE('',#12553,#2348);
#2000=LINE('',#12555,#2349);
#2001=LINE('',#12557,#2350);
#2002=LINE('',#12559,#2351);
#2003=LINE('',#12561,#2352);
#2004=LINE('',#12563,#2353);
#2005=LINE('',#12565,#2354);
#2006=LINE('',#12567,#2355);
#2007=LINE('',#12569,#2356);
#2008=LINE('',#12571,#2357);
#2009=LINE('',#12573,#2358);
#2010=LINE('',#12575,#2359);
#2011=LINE('',#12577,#2360);
#2012=LINE('',#12579,#2361);
#2013=LINE('',#12581,#2362);
#2014=LINE('',#12583,#2363);
#2015=LINE('',#12585,#2364);
#2016=LINE('',#12587,#2365);
#2017=LINE('',#12589,#2366);
#2018=LINE('',#12591,#2367);
#2019=LINE('',#12593,#2368);
#2020=LINE('',#12595,#2369);
#2021=LINE('',#12597,#2370);
#2022=LINE('',#12599,#2371);
#2023=LINE('',#12601,#2372);
#2024=LINE('',#12603,#2373);
#2025=LINE('',#12605,#2374);
#2026=LINE('',#12607,#2375);
#2027=LINE('',#12609,#2376);
#2028=LINE('',#12611,#2377);
#2029=LINE('',#12613,#2378);
#2030=LINE('',#12615,#2379);
#2031=LINE('',#12617,#2380);
#2032=LINE('',#12619,#2381);
#2033=LINE('',#12625,#2382);
#2034=LINE('',#12627,#2383);
#2035=LINE('',#12629,#2384);
#2036=LINE('',#12630,#2385);
#2037=LINE('',#12633,#2386);
#2038=LINE('',#12635,#2387);
#2039=LINE('',#12636,#2388);
#2040=LINE('',#12639,#2389);
#2041=LINE('',#12641,#2390);
#2042=LINE('',#12642,#2391);
#2043=LINE('',#12645,#2392);
#2044=LINE('',#12647,#2393);
#2045=LINE('',#12648,#2394);
#2046=LINE('',#12651,#2395);
#2047=LINE('',#12653,#2396);
#2048=LINE('',#12654,#2397);
#2049=LINE('',#12656,#2398);
#2050=LINE('',#12657,#2399);
#2051=LINE('',#12669,#2400);
#2052=LINE('',#12673,#2401);
#2053=LINE('',#12677,#2402);
#2054=LINE('',#12684,#2403);
#2055=LINE('',#12686,#2404);
#2056=VECTOR('',#7443,0.225);
#2057=VECTOR('',#7450,0.225);
#2058=VECTOR('',#7457,0.21);
#2059=VECTOR('',#7464,0.21);
#2060=VECTOR('',#7471,0.21);
#2061=VECTOR('',#7476,1.);
#2062=VECTOR('',#7477,1.);
#2063=VECTOR('',#7478,1.);
#2064=VECTOR('',#7479,1.);
#2065=VECTOR('',#7482,1.);
#2066=VECTOR('',#7483,1.);
#2067=VECTOR('',#7484,1.);
#2068=VECTOR('',#7487,1.);
#2069=VECTOR('',#7488,1.);
#2070=VECTOR('',#7489,1.);
#2071=VECTOR('',#7492,1.);
#2072=VECTOR('',#7493,1.);
#2073=VECTOR('',#7502,1.);
#2074=VECTOR('',#7503,1.);
#2075=VECTOR('',#7504,1.);
#2076=VECTOR('',#7505,1.);
#2077=VECTOR('',#7508,1.);
#2078=VECTOR('',#7509,1.);
#2079=VECTOR('',#7510,1.);
#2080=VECTOR('',#7513,1.);
#2081=VECTOR('',#7514,1.);
#2082=VECTOR('',#7515,1.);
#2083=VECTOR('',#7518,1.);
#2084=VECTOR('',#7519,1.);
#2085=VECTOR('',#7528,1.);
#2086=VECTOR('',#7529,1.);
#2087=VECTOR('',#7530,1.);
#2088=VECTOR('',#7531,1.);
#2089=VECTOR('',#7534,1.);
#2090=VECTOR('',#7535,1.);
#2091=VECTOR('',#7536,1.);
#2092=VECTOR('',#7539,1.);
#2093=VECTOR('',#7540,1.);
#2094=VECTOR('',#7541,1.);
#2095=VECTOR('',#7544,1.);
#2096=VECTOR('',#7545,1.);
#2097=VECTOR('',#7556,0.275);
#2098=VECTOR('',#7563,0.275);
#2099=VECTOR('',#7570,0.275);
#2100=VECTOR('',#7581,0.7);
#2101=VECTOR('',#7588,0.5);
#2102=VECTOR('',#7599,2.8);
#2103=VECTOR('',#7606,1.2);
#2104=VECTOR('',#7615,1.);
#2105=VECTOR('',#7622,0.165);
#2106=VECTOR('',#7625,1.);
#2107=VECTOR('',#7630,0.505);
#2108=VECTOR('',#7637,0.9);
#2109=VECTOR('',#7650,0.165);
#2110=VECTOR('',#7657,0.07);
#2111=VECTOR('',#7662,0.5);
#2112=VECTOR('',#7675,0.0599999999999996);
#2113=VECTOR('',#7684,1.);
#2114=VECTOR('',#7695,0.0600000000000001);
#2115=VECTOR('',#7698,1.);
#2116=VECTOR('',#7711,0.06);
#2117=VECTOR('',#7716,1.);
#2118=VECTOR('',#7727,0.165);
#2119=VECTOR('',#7736,0.21);
#2120=VECTOR('',#7741,1.);
#2121=VECTOR('',#7742,1.);
#2122=VECTOR('',#7743,1.);
#2123=VECTOR('',#7744,1.);
#2124=VECTOR('',#7747,1.);
#2125=VECTOR('',#7748,1.);
#2126=VECTOR('',#7749,1.);
#2127=VECTOR('',#7752,1.);
#2128=VECTOR('',#7753,1.);
#2129=VECTOR('',#7754,1.);
#2130=VECTOR('',#7757,1.);
#2131=VECTOR('',#7758,1.);
#2132=VECTOR('',#7769,0.275);
#2133=VECTOR('',#7774,0.265);
#2134=VECTOR('',#7783,0.5);
#2135=VECTOR('',#7798,0.4);
#2136=VECTOR('',#7803,0.425);
#2137=VECTOR('',#7808,0.41);
#2138=VECTOR('',#7817,0.26);
#2139=VECTOR('',#7822,0.25);
#2140=VECTOR('',#7827,0.225);
#2141=VECTOR('',#7832,1.);
#2142=VECTOR('',#7833,1.);
#2143=VECTOR('',#7834,1.);
#2144=VECTOR('',#7835,1.);
#2145=VECTOR('',#7838,1.);
#2146=VECTOR('',#7839,1.);
#2147=VECTOR('',#7840,1.);
#2148=VECTOR('',#7843,1.);
#2149=VECTOR('',#7844,1.);
#2150=VECTOR('',#7845,1.);
#2151=VECTOR('',#7848,1.);
#2152=VECTOR('',#7849,1.);
#2153=VECTOR('',#7850,1.);
#2154=VECTOR('',#7853,1.);
#2155=VECTOR('',#7854,1.);
#2156=VECTOR('',#7855,1.);
#2157=VECTOR('',#7858,1.);
#2158=VECTOR('',#7859,1.);
#2159=VECTOR('',#7868,0.47094010767585);
#2160=VECTOR('',#7875,0.47094010767585);
#2161=VECTOR('',#7878,1.);
#2162=VECTOR('',#7879,1.);
#2163=VECTOR('',#7882,1.);
#2164=VECTOR('',#7885,1.);
#2165=VECTOR('',#7890,0.25);
#2166=VECTOR('',#7895,1.);
#2167=VECTOR('',#7898,1.);
#2168=VECTOR('',#7915,0.325);
#2169=VECTOR('',#7920,0.35);
#2170=VECTOR('',#7925,0.335);
#2171=VECTOR('',#7934,0.21);
#2172=VECTOR('',#7939,0.2);
#2173=VECTOR('',#7944,0.18);
#2174=VECTOR('',#7949,1.);
#2175=VECTOR('',#7950,1.);
#2176=VECTOR('',#7951,1.);
#2177=VECTOR('',#7952,1.);
#2178=VECTOR('',#7955,1.);
#2179=VECTOR('',#7956,1.);
#2180=VECTOR('',#7957,1.);
#2181=VECTOR('',#7960,1.);
#2182=VECTOR('',#7961,1.);
#2183=VECTOR('',#7962,1.);
#2184=VECTOR('',#7965,1.);
#2185=VECTOR('',#7966,1.);
#2186=VECTOR('',#7967,1.);
#2187=VECTOR('',#7970,1.);
#2188=VECTOR('',#7971,1.);
#2189=VECTOR('',#7972,1.);
#2190=VECTOR('',#7975,1.);
#2191=VECTOR('',#7976,1.);
#2192=VECTOR('',#7989,0.165);
#2193=VECTOR('',#7996,0.165);
#2194=VECTOR('',#8003,0.164999999999999);
#2195=VECTOR('',#8010,0.164999999999999);
#2196=VECTOR('',#8017,0.165);
#2197=VECTOR('',#8024,0.165);
#2198=VECTOR('',#8031,0.165);
#2199=VECTOR('',#8038,0.165);
#2200=VECTOR('',#8045,1.5);
#2201=VECTOR('',#8052,1.5);
#2202=VECTOR('',#8057,1.);
#2203=VECTOR('',#8060,1.);
#2204=VECTOR('',#8065,1.);
#2205=VECTOR('',#8066,1.);
#2206=VECTOR('',#8067,1.);
#2207=VECTOR('',#8070,1.);
#2208=VECTOR('',#8075,1.);
#2209=VECTOR('',#8076,1.);
#2210=VECTOR('',#8089,0.225);
#2211=VECTOR('',#8096,0.225);
#2212=VECTOR('',#8103,0.225);
#2213=VECTOR('',#8110,0.225);
#2214=VECTOR('',#8117,1.49);
#2215=VECTOR('',#8126,1.02);
#2216=VECTOR('',#8133,2.);
#2217=VECTOR('',#8146,0.225);
#2218=VECTOR('',#8153,0.225);
#2219=VECTOR('',#8160,0.225);
#2220=VECTOR('',#8167,0.225);
#2221=VECTOR('',#8174,1.49);
#2222=VECTOR('',#8185,1.02);
#2223=VECTOR('',#8190,2.);
#2224=VECTOR('',#8203,0.225);
#2225=VECTOR('',#8210,0.225);
#2226=VECTOR('',#8217,0.225);
#2227=VECTOR('',#8224,0.225);
#2228=VECTOR('',#8231,1.49);
#2229=VECTOR('',#8240,1.02);
#2230=VECTOR('',#8247,2.);
#2231=VECTOR('',#8260,0.225);
#2232=VECTOR('',#8267,0.225);
#2233=VECTOR('',#8274,0.225);
#2234=VECTOR('',#8281,0.225);
#2235=VECTOR('',#8288,1.49);
#2236=VECTOR('',#8299,1.02);
#2237=VECTOR('',#8304,2.);
#2238=VECTOR('',#8315,0.0700000000000003);
#2239=VECTOR('',#8320,0.5);
#2240=VECTOR('',#8321,0.5);
#2241=VECTOR('',#8332,1.);
#2242=VECTOR('',#8333,1.);
#2243=VECTOR('',#8336,1.);
#2244=VECTOR('',#8337,1.);
#2245=VECTOR('',#8340,1.);
#2246=VECTOR('',#8341,1.);
#2247=VECTOR('',#8342,1.);
#2248=VECTOR('',#8345,1.);
#2249=VECTOR('',#8346,1.);
#2250=VECTOR('',#8347,1.);
#2251=VECTOR('',#8350,1.);
#2252=VECTOR('',#8351,1.);
#2253=VECTOR('',#8354,1.);
#2254=VECTOR('',#8355,1.);
#2255=VECTOR('',#8358,1.);
#2256=VECTOR('',#8379,0.976185);
#2257=VECTOR('',#8386,0.5);
#2258=VECTOR('',#8391,0.53);
#2259=VECTOR('',#8400,0.976185);
#2260=VECTOR('',#8407,0.53);
#2261=VECTOR('',#8426,1.023815);
#2262=VECTOR('',#8437,1.47);
#2263=VECTOR('',#8442,1.5);
#2264=VECTOR('',#8447,1.47);
#2265=VECTOR('',#8452,1.023815);
#2266=VECTOR('',#8503,1.019052);
#2267=VECTOR('',#8580,0.980948);
#2268=VECTOR('',#8609,1.013815);
#2269=VECTOR('',#8616,0.991185);
#2270=VECTOR('',#8627,1.013815);
#2271=VECTOR('',#8634,0.991185);
#2272=VECTOR('',#8659,0.325);
#2273=VECTOR('',#8664,0.35);
#2274=VECTOR('',#8669,0.335);
#2275=VECTOR('',#8678,0.21);
#2276=VECTOR('',#8681,0.2);
#2277=VECTOR('',#8684,1.);
#2278=VECTOR('',#8685,1.);
#2279=VECTOR('',#8686,1.);
#2280=VECTOR('',#8687,1.);
#2281=VECTOR('',#8690,1.);
#2282=VECTOR('',#8691,1.);
#2283=VECTOR('',#8692,1.);
#2284=VECTOR('',#8695,1.);
#2285=VECTOR('',#8696,1.);
#2286=VECTOR('',#8697,1.);
#2287=VECTOR('',#8700,1.);
#2288=VECTOR('',#8701,1.);
#2289=VECTOR('',#8702,1.);
#2290=VECTOR('',#8705,1.);
#2291=VECTOR('',#8706,1.);
#2292=VECTOR('',#8707,1.);
#2293=VECTOR('',#8710,1.);
#2294=VECTOR('',#8711,1.);
#2295=VECTOR('',#8772,0.164999999999999);
#2296=VECTOR('',#8781,0.4);
#2297=VECTOR('',#8796,0.699999999999999);
#2298=VECTOR('',#8799,0.5);
#2299=VECTOR('',#8810,1.);
#2300=VECTOR('',#8817,0.165);
#2301=VECTOR('',#8820,1.);
#2302=VECTOR('',#8825,0.505000000000001);
#2303=VECTOR('',#8832,0.9);
#2304=VECTOR('',#8845,0.404999999999999);
#2305=VECTOR('',#8852,0.6);
#2306=VECTOR('',#8865,0.404999999999999);
#2307=VECTOR('',#8872,0.6);
#2308=VECTOR('',#8885,0.15);
#2309=VECTOR('',#8898,0.15);
#2310=VECTOR('',#8911,0.225);
#2311=VECTOR('',#8918,0.6);
#2312=VECTOR('',#8933,1.);
#2313=VECTOR('',#8934,1.);
#2314=VECTOR('',#8935,1.);
#2315=VECTOR('',#8936,1.);
#2316=VECTOR('',#8939,1.);
#2317=VECTOR('',#8940,1.);
#2318=VECTOR('',#8941,1.);
#2319=VECTOR('',#8944,1.);
#2320=VECTOR('',#8945,1.);
#2321=VECTOR('',#8946,1.);
#2322=VECTOR('',#8949,1.);
#2323=VECTOR('',#8950,1.);
#2324=VECTOR('',#8951,1.);
#2325=VECTOR('',#8954,1.);
#2326=VECTOR('',#8955,1.);
#2327=VECTOR('',#8956,1.);
#2328=VECTOR('',#8959,1.);
#2329=VECTOR('',#8960,1.);
#2330=VECTOR('',#8971,0.185);
#2331=VECTOR('',#8974,0.2);
#2332=VECTOR('',#9017,0.125);
#2333=VECTOR('',#9020,0.125);
#2334=VECTOR('',#9025,0.65);
#2335=VECTOR('',#9026,0.65);
#2336=VECTOR('',#9031,0.125);
#2337=VECTOR('',#9034,0.125);
#2338=VECTOR('',#9039,0.4);
#2339=VECTOR('',#9040,0.4);
#2340=VECTOR('',#9133,0.8);
#2341=VECTOR('',#9224,0.8);
#2342=VECTOR('',#9229,1.);
#2343=VECTOR('',#9230,1.);
#2344=VECTOR('',#9233,1.);
#2345=VECTOR('',#9236,1.);
#2346=VECTOR('',#9239,1.);
#2347=VECTOR('',#9242,1.);
#2348=VECTOR('',#9245,1.);
#2349=VECTOR('',#9248,1.);
#2350=VECTOR('',#9251,1.);
#2351=VECTOR('',#9254,1.);
#2352=VECTOR('',#9257,1.);
#2353=VECTOR('',#9260,1.);
#2354=VECTOR('',#9263,1.);
#2355=VECTOR('',#9266,1.);
#2356=VECTOR('',#9269,1.);
#2357=VECTOR('',#9272,1.);
#2358=VECTOR('',#9275,1.);
#2359=VECTOR('',#9278,1.);
#2360=VECTOR('',#9281,1.);
#2361=VECTOR('',#9284,1.);
#2362=VECTOR('',#9287,1.);
#2363=VECTOR('',#9290,1.);
#2364=VECTOR('',#9293,1.);
#2365=VECTOR('',#9296,1.);
#2366=VECTOR('',#9299,1.);
#2367=VECTOR('',#9302,1.);
#2368=VECTOR('',#9305,1.);
#2369=VECTOR('',#9308,1.);
#2370=VECTOR('',#9311,1.);
#2371=VECTOR('',#9314,1.);
#2372=VECTOR('',#9317,1.);
#2373=VECTOR('',#9320,1.);
#2374=VECTOR('',#9323,1.);
#2375=VECTOR('',#9326,1.);
#2376=VECTOR('',#9329,1.);
#2377=VECTOR('',#9332,1.);
#2378=VECTOR('',#9335,1.);
#2379=VECTOR('',#9338,1.);
#2380=VECTOR('',#9341,1.);
#2381=VECTOR('',#9344,1.);
#2382=VECTOR('',#9351,1.);
#2383=VECTOR('',#9352,1.);
#2384=VECTOR('',#9353,1.);
#2385=VECTOR('',#9354,1.);
#2386=VECTOR('',#9357,1.);
#2387=VECTOR('',#9358,1.);
#2388=VECTOR('',#9359,1.);
#2389=VECTOR('',#9362,1.);
#2390=VECTOR('',#9363,1.);
#2391=VECTOR('',#9364,1.);
#2392=VECTOR('',#9367,1.);
#2393=VECTOR('',#9368,1.);
#2394=VECTOR('',#9369,1.);
#2395=VECTOR('',#9372,1.);
#2396=VECTOR('',#9373,1.);
#2397=VECTOR('',#9374,1.);
#2398=VECTOR('',#9377,1.);
#2399=VECTOR('',#9378,1.);
#2400=VECTOR('',#9395,0.325);
#2401=VECTOR('',#9400,0.35);
#2402=VECTOR('',#9405,0.335);
#2403=VECTOR('',#9414,0.21);
#2404=VECTOR('',#9417,0.2);
#2405=CIRCLE('',#6606,0.225);
#2406=CIRCLE('',#6607,0.225);
#2407=CIRCLE('',#6609,0.225);
#2408=CIRCLE('',#6610,0.225);
#2409=CIRCLE('',#6612,0.21);
#2410=CIRCLE('',#6613,0.21);
#2411=CIRCLE('',#6615,0.21);
#2412=CIRCLE('',#6616,0.21);
#2413=CIRCLE('',#6618,0.21);
#2414=CIRCLE('',#6619,0.21);
#2415=CIRCLE('',#6642,0.275);
#2416=CIRCLE('',#6643,0.275);
#2417=CIRCLE('',#6645,0.275);
#2418=CIRCLE('',#6646,0.275);
#2419=CIRCLE('',#6648,0.275);
#2420=CIRCLE('',#6649,0.275);
#2421=CIRCLE('',#6651,0.7);
#2422=CIRCLE('',#6652,0.5);
#2423=CIRCLE('',#6654,0.7);
#2424=CIRCLE('',#6656,0.5);
#2425=CIRCLE('',#6659,2.8);
#2426=CIRCLE('',#6660,1.2);
#2427=CIRCLE('',#6662,2.8);
#2428=CIRCLE('',#6664,1.2);
#2429=CIRCLE('',#6669,0.165);
#2430=CIRCLE('',#6671,0.165);
#2431=CIRCLE('',#6674,0.505);
#2432=CIRCLE('',#6675,0.505);
#2433=CIRCLE('',#6677,0.9);
#2434=CIRCLE('',#6678,0.9);
#2435=CIRCLE('',#6683,0.165);
#2436=CIRCLE('',#6684,0.165);
#2437=CIRCLE('',#6688,0.5);
#2438=CIRCLE('',#6689,0.5);
#2439=CIRCLE('',#6694,0.0599999999999996);
#2440=CIRCLE('',#6696,0.0599999999999996);
#2441=CIRCLE('',#6700,0.0600000000000001);
#2442=CIRCLE('',#6701,0.0600000000000001);
#2443=CIRCLE('',#6703,0.0600000000000001);
#2444=CIRCLE('',#6706,0.06);
#2445=CIRCLE('',#6707,0.06);
#2446=CIRCLE('',#6708,0.06);
#2447=CIRCLE('',#6710,0.0600000000000001);
#2448=CIRCLE('',#6711,0.0600000000000001);
#2449=CIRCLE('',#6717,0.165);
#2450=CIRCLE('',#6718,0.165);
#2451=CIRCLE('',#6721,0.21);
#2452=CIRCLE('',#6722,0.21);
#2453=CIRCLE('',#6731,0.285);
#2454=CIRCLE('',#6732,0.265);
#2455=CIRCLE('',#6734,0.265);
#2456=CIRCLE('',#6736,0.5);
#2457=CIRCLE('',#6738,0.5);
#2458=CIRCLE('',#6742,0.375);
#2459=CIRCLE('',#6744,0.425);
#2460=CIRCLE('',#6746,0.425);
#2461=CIRCLE('',#6748,0.395);
#2462=CIRCLE('',#6750,0.27);
#2463=CIRCLE('',#6752,0.24505);
#2464=CIRCLE('',#6754,0.24505);
#2465=CIRCLE('',#6756,0.2);
#2466=CIRCLE('',#6768,0.38);
#2467=CIRCLE('',#6770,0.38);
#2468=CIRCLE('',#6775,0.2117);
#2469=CIRCLE('',#6776,0.2117);
#2470=CIRCLE('',#6784,0.3);
#2471=CIRCLE('',#6786,0.35);
#2472=CIRCLE('',#6788,0.35);
#2473=CIRCLE('',#6790,0.32);
#2474=CIRCLE('',#6792,0.22);
#2475=CIRCLE('',#6794,0.1954);
#2476=CIRCLE('',#6796,0.1954);
#2477=CIRCLE('',#6798,0.16);
#2478=CIRCLE('',#6811,0.165);
#2479=CIRCLE('',#6812,0.165);
#2480=CIRCLE('',#6814,0.165);
#2481=CIRCLE('',#6815,0.165);
#2482=CIRCLE('',#6817,0.164999999999999);
#2483=CIRCLE('',#6818,0.164999999999999);
#2484=CIRCLE('',#6820,0.164999999999999);
#2485=CIRCLE('',#6821,0.164999999999999);
#2486=CIRCLE('',#6823,0.165);
#2487=CIRCLE('',#6824,0.165);
#2488=CIRCLE('',#6826,0.165);
#2489=CIRCLE('',#6827,0.165);
#2490=CIRCLE('',#6829,0.165);
#2491=CIRCLE('',#6830,0.165);
#2492=CIRCLE('',#6832,0.165);
#2493=CIRCLE('',#6833,0.165);
#2494=CIRCLE('',#6835,1.5);
#2495=CIRCLE('',#6836,1.5);
#2496=CIRCLE('',#6838,1.5);
#2497=CIRCLE('',#6839,1.5);
#2498=CIRCLE('',#6841,2.);
#2499=CIRCLE('',#6842,2.);
#2500=CIRCLE('',#6845,2.);
#2501=CIRCLE('',#6848,2.);
#2502=CIRCLE('',#6852,0.225);
#2503=CIRCLE('',#6853,0.225);
#2504=CIRCLE('',#6855,0.225);
#2505=CIRCLE('',#6856,0.225);
#2506=CIRCLE('',#6858,0.225);
#2507=CIRCLE('',#6859,0.225);
#2508=CIRCLE('',#6861,0.225);
#2509=CIRCLE('',#6862,0.225);
#2510=CIRCLE('',#6864,1.49);
#2511=CIRCLE('',#6865,1.49);
#2512=CIRCLE('',#6867,1.02);
#2513=CIRCLE('',#6869,1.02);
#2514=CIRCLE('',#6871,2.);
#2515=CIRCLE('',#6872,2.);
#2516=CIRCLE('',#6877,0.225);
#2517=CIRCLE('',#6878,0.225);
#2518=CIRCLE('',#6880,0.225);
#2519=CIRCLE('',#6881,0.225);
#2520=CIRCLE('',#6883,0.225);
#2521=CIRCLE('',#6884,0.225);
#2522=CIRCLE('',#6886,0.225);
#2523=CIRCLE('',#6887,0.225);
#2524=CIRCLE('',#6889,1.49);
#2525=CIRCLE('',#6890,1.49);
#2526=CIRCLE('',#6892,1.02);
#2527=CIRCLE('',#6894,1.02);
#2528=CIRCLE('',#6896,2.);
#2529=CIRCLE('',#6897,2.);
#2530=CIRCLE('',#6902,0.225);
#2531=CIRCLE('',#6903,0.225);
#2532=CIRCLE('',#6905,0.225);
#2533=CIRCLE('',#6906,0.225);
#2534=CIRCLE('',#6908,0.225);
#2535=CIRCLE('',#6909,0.225);
#2536=CIRCLE('',#6911,0.225);
#2537=CIRCLE('',#6912,0.225);
#2538=CIRCLE('',#6914,1.49);
#2539=CIRCLE('',#6915,1.49);
#2540=CIRCLE('',#6917,1.02);
#2541=CIRCLE('',#6919,1.02);
#2542=CIRCLE('',#6921,2.);
#2543=CIRCLE('',#6922,2.);
#2544=CIRCLE('',#6927,0.225);
#2545=CIRCLE('',#6928,0.225);
#2546=CIRCLE('',#6930,0.225);
#2547=CIRCLE('',#6931,0.225);
#2548=CIRCLE('',#6933,0.225);
#2549=CIRCLE('',#6934,0.225);
#2550=CIRCLE('',#6936,0.225);
#2551=CIRCLE('',#6937,0.225);
#2552=CIRCLE('',#6939,1.49);
#2553=CIRCLE('',#6940,1.49);
#2554=CIRCLE('',#6942,1.02);
#2555=CIRCLE('',#6944,1.02);
#2556=CIRCLE('',#6946,2.);
#2557=CIRCLE('',#6947,2.);
#2558=CIRCLE('',#6953,0.5);
#2559=CIRCLE('',#6954,0.5);
#2560=CIRCLE('',#6955,0.5);
#2561=CIRCLE('',#6956,0.5);
#2562=CIRCLE('',#6969,0.976185);
#2563=CIRCLE('',#6970,0.976185);
#2564=CIRCLE('',#6971,0.247676);
#2565=CIRCLE('',#6972,0.976185);
#2566=CIRCLE('',#6973,0.976185);
#2567=CIRCLE('',#6975,0.976185);
#2568=CIRCLE('',#6977,0.5);
#2569=CIRCLE('',#6978,0.5);
#2570=CIRCLE('',#6980,0.56);
#2571=CIRCLE('',#6983,0.976185);
#2572=CIRCLE('',#6985,0.56);
#2573=CIRCLE('',#6989,1.023815);
#2574=CIRCLE('',#6990,1.023815);
#2575=CIRCLE('',#6991,0.247676);
#2576=CIRCLE('',#6992,1.023815);
#2577=CIRCLE('',#6993,1.023815);
#2578=CIRCLE('',#6995,1.023815);
#2579=CIRCLE('',#6997,1.44);
#2580=CIRCLE('',#6998,1.023815);
#2581=CIRCLE('',#7000,1.5);
#2582=CIRCLE('',#7002,1.5);
#2583=CIRCLE('',#7004,1.44);
#2584=CIRCLE('',#7009,0.23815);
#2585=CIRCLE('',#7011,0.23815);
#2586=CIRCLE('',#7013,0.23815);
#2587=CIRCLE('',#7015,0.23815);
#2588=CIRCLE('',#7017,0.23815);
#2589=CIRCLE('',#7019,0.23815);
#2590=CIRCLE('',#7021,0.23815);
#2591=CIRCLE('',#7023,0.23815);
#2592=CIRCLE('',#7026,0.243053047864041);
#2593=CIRCLE('',#7027,0.243053047864041);
#2594=CIRCLE('',#7029,1.019052);
#2595=CIRCLE('',#7030,1.019052);
#2596=CIRCLE('',#7031,1.019052);
#2597=CIRCLE('',#7032,1.019052);
#2598=CIRCLE('',#7033,1.019052);
#2599=CIRCLE('',#7034,1.019052);
#2600=CIRCLE('',#7035,1.019052);
#2601=CIRCLE('',#7036,1.019052);
#2602=CIRCLE('',#7037,1.019052);
#2603=CIRCLE('',#7039,0.980948);
#2604=CIRCLE('',#7040,0.243053047864041);
#2605=CIRCLE('',#7042,0.243053047864041);
#2606=CIRCLE('',#7044,0.980948);
#2607=CIRCLE('',#7045,0.243053047864041);
#2608=CIRCLE('',#7047,0.243053047864041);
#2609=CIRCLE('',#7049,0.980948);
#2610=CIRCLE('',#7050,0.243053047864041);
#2611=CIRCLE('',#7052,0.243053047864041);
#2612=CIRCLE('',#7054,0.980948);
#2613=CIRCLE('',#7055,0.243053047864041);
#2614=CIRCLE('',#7057,0.243053047864041);
#2615=CIRCLE('',#7059,0.980948);
#2616=CIRCLE('',#7060,0.243053047864041);
#2617=CIRCLE('',#7062,0.243053047864041);
#2618=CIRCLE('',#7064,0.980948);
#2619=CIRCLE('',#7065,0.243053047864041);
#2620=CIRCLE('',#7067,0.243053047864041);
#2621=CIRCLE('',#7069,0.980948);
#2622=CIRCLE('',#7070,0.980948);
#2623=CIRCLE('',#7071,0.980948);
#2624=CIRCLE('',#7073,0.243053047864041);
#2625=CIRCLE('',#7075,0.243053047864041);
#2626=CIRCLE('',#7080,1.013815);
#2627=CIRCLE('',#7081,0.991185);
#2628=CIRCLE('',#7083,1.013815);
#2629=CIRCLE('',#7085,0.991185);
#2630=CIRCLE('',#7088,1.013815);
#2631=CIRCLE('',#7089,0.991185);
#2632=CIRCLE('',#7091,1.013815);
#2633=CIRCLE('',#7093,0.991185);
#2634=CIRCLE('',#7102,0.1954);
#2635=CIRCLE('',#7104,0.3);
#2636=CIRCLE('',#7106,0.35);
#2637=CIRCLE('',#7108,0.35);
#2638=CIRCLE('',#7110,0.32);
#2639=CIRCLE('',#7112,0.22);
#2640=CIRCLE('',#7114,0.1954);
#2641=CIRCLE('',#7151,0.164999999999999);
#2642=CIRCLE('',#7152,0.164999999999999);
#2643=CIRCLE('',#7155,0.4);
#2644=CIRCLE('',#7156,0.4);
#2645=CIRCLE('',#7159,0.699999999999999);
#2646=CIRCLE('',#7160,0.5);
#2647=CIRCLE('',#7162,0.699999999999999);
#2648=CIRCLE('',#7164,0.5);
#2649=CIRCLE('',#7169,0.165);
#2650=CIRCLE('',#7171,0.165);
#2651=CIRCLE('',#7174,0.505000000000001);
#2652=CIRCLE('',#7175,0.505000000000001);
#2653=CIRCLE('',#7177,0.9);
#2654=CIRCLE('',#7178,0.9);
#2655=CIRCLE('',#7183,0.404999999999999);
#2656=CIRCLE('',#7184,0.404999999999999);
#2657=CIRCLE('',#7186,0.6);
#2658=CIRCLE('',#7187,0.6);
#2659=CIRCLE('',#7192,0.404999999999999);
#2660=CIRCLE('',#7193,0.404999999999999);
#2661=CIRCLE('',#7195,0.6);
#2662=CIRCLE('',#7196,0.6);
#2663=CIRCLE('',#7201,0.15);
#2664=CIRCLE('',#7202,0.15);
#2665=CIRCLE('',#7207,0.15);
#2666=CIRCLE('',#7208,0.15);
#2667=CIRCLE('',#7213,0.225);
#2668=CIRCLE('',#7214,0.225);
#2669=CIRCLE('',#7216,0.6);
#2670=CIRCLE('',#7217,0.6);
#2671=CIRCLE('',#7222,0.1954);
#2672=CIRCLE('',#7231,0.17);
#2673=CIRCLE('',#7233,0.1954);
#2674=CIRCLE('',#7258,0.65);
#2675=CIRCLE('',#7259,0.65);
#2676=CIRCLE('',#7263,0.4);
#2677=CIRCLE('',#7264,0.4);
#2678=CIRCLE('',#7267,0.8);
#2679=CIRCLE('',#7268,0.0555);
#2680=CIRCLE('',#7269,0.611219772367581);
#2681=CIRCLE('',#7270,0.0555);
#2682=CIRCLE('',#7271,0.611219772367581);
#2683=CIRCLE('',#7272,0.0555);
#2684=CIRCLE('',#7273,0.611219772367581);
#2685=CIRCLE('',#7274,0.0555);
#2686=CIRCLE('',#7275,0.611219772367581);
#2687=CIRCLE('',#7276,0.0555);
#2688=CIRCLE('',#7277,0.611219772367581);
#2689=CIRCLE('',#7278,0.0555);
#2690=CIRCLE('',#7279,0.611219772367581);
#2691=CIRCLE('',#7280,0.0555);
#2692=CIRCLE('',#7281,0.611219772367581);
#2693=CIRCLE('',#7282,0.0555);
#2694=CIRCLE('',#7283,0.611219772367581);
#2695=CIRCLE('',#7284,0.0555);
#2696=CIRCLE('',#7285,0.611219772367581);
#2697=CIRCLE('',#7286,0.0555);
#2698=CIRCLE('',#7287,0.611219772367581);
#2699=CIRCLE('',#7288,0.0555);
#2700=CIRCLE('',#7289,0.611219772367581);
#2701=CIRCLE('',#7290,0.0555);
#2702=CIRCLE('',#7291,0.611219772367581);
#2703=CIRCLE('',#7292,0.0555);
#2704=CIRCLE('',#7293,0.611219772367581);
#2705=CIRCLE('',#7294,0.0555);
#2706=CIRCLE('',#7295,0.611219772367581);
#2707=CIRCLE('',#7296,0.0555);
#2708=CIRCLE('',#7297,0.611219772367581);
#2709=CIRCLE('',#7298,0.0555);
#2710=CIRCLE('',#7299,0.611219772367581);
#2711=CIRCLE('',#7300,0.0555);
#2712=CIRCLE('',#7301,0.611219772367581);
#2713=CIRCLE('',#7302,0.0555);
#2714=CIRCLE('',#7303,0.611219772367581);
#2715=CIRCLE('',#7304,0.0555);
#2716=CIRCLE('',#7305,0.611219772367581);
#2717=CIRCLE('',#7306,0.0555);
#2718=CIRCLE('',#7307,0.611219772367581);
#2719=CIRCLE('',#7309,0.8);
#2720=CIRCLE('',#7312,0.8);
#2721=CIRCLE('',#7313,0.0555);
#2722=CIRCLE('',#7314,0.611219772367581);
#2723=CIRCLE('',#7315,0.0555);
#2724=CIRCLE('',#7316,0.611219772367581);
#2725=CIRCLE('',#7317,0.0555);
#2726=CIRCLE('',#7318,0.611219772367581);
#2727=CIRCLE('',#7319,0.0555);
#2728=CIRCLE('',#7320,0.611219772367581);
#2729=CIRCLE('',#7321,0.0555);
#2730=CIRCLE('',#7322,0.611219772367581);
#2731=CIRCLE('',#7323,0.0555);
#2732=CIRCLE('',#7324,0.611219772367581);
#2733=CIRCLE('',#7325,0.0555);
#2734=CIRCLE('',#7326,0.611219772367581);
#2735=CIRCLE('',#7327,0.0555);
#2736=CIRCLE('',#7328,0.611219772367581);
#2737=CIRCLE('',#7329,0.0555);
#2738=CIRCLE('',#7330,0.611219772367581);
#2739=CIRCLE('',#7331,0.0555);
#2740=CIRCLE('',#7332,0.611219772367581);
#2741=CIRCLE('',#7333,0.0555);
#2742=CIRCLE('',#7334,0.611219772367581);
#2743=CIRCLE('',#7335,0.0555);
#2744=CIRCLE('',#7336,0.611219772367581);
#2745=CIRCLE('',#7337,0.0555);
#2746=CIRCLE('',#7338,0.611219772367581);
#2747=CIRCLE('',#7339,0.0555);
#2748=CIRCLE('',#7340,0.611219772367581);
#2749=CIRCLE('',#7341,0.0555);
#2750=CIRCLE('',#7342,0.611219772367581);
#2751=CIRCLE('',#7343,0.0555);
#2752=CIRCLE('',#7344,0.611219772367581);
#2753=CIRCLE('',#7345,0.0555);
#2754=CIRCLE('',#7346,0.611219772367581);
#2755=CIRCLE('',#7347,0.0555);
#2756=CIRCLE('',#7348,0.611219772367581);
#2757=CIRCLE('',#7349,0.0555);
#2758=CIRCLE('',#7350,0.611219772367581);
#2759=CIRCLE('',#7351,0.0555);
#2760=CIRCLE('',#7352,0.611219772367581);
#2761=CIRCLE('',#7354,0.8);
#2762=CIRCLE('',#7406,0.1954);
#2763=CIRCLE('',#7408,0.3);
#2764=CIRCLE('',#7410,0.35);
#2765=CIRCLE('',#7412,0.35);
#2766=CIRCLE('',#7414,0.32);
#2767=CIRCLE('',#7416,0.22);
#2768=CIRCLE('',#7418,0.1954);
#2769=VERTEX_POINT('',#9448);
#2770=VERTEX_POINT('',#9450);
#2771=VERTEX_POINT('',#9454);
#2772=VERTEX_POINT('',#9456);
#2773=VERTEX_POINT('',#9460);
#2774=VERTEX_POINT('',#9462);
#2775=VERTEX_POINT('',#9466);
#2776=VERTEX_POINT('',#9468);
#2777=VERTEX_POINT('',#9472);
#2778=VERTEX_POINT('',#9474);
#2779=VERTEX_POINT('',#9478);
#2780=VERTEX_POINT('',#9479);
#2781=VERTEX_POINT('',#9481);
#2782=VERTEX_POINT('',#9483);
#2783=VERTEX_POINT('',#9487);
#2784=VERTEX_POINT('',#9489);
#2785=VERTEX_POINT('',#9493);
#2786=VERTEX_POINT('',#9495);
#2787=VERTEX_POINT('',#9505);
#2788=VERTEX_POINT('',#9506);
#2789=VERTEX_POINT('',#9508);
#2790=VERTEX_POINT('',#9510);
#2791=VERTEX_POINT('',#9514);
#2792=VERTEX_POINT('',#9516);
#2793=VERTEX_POINT('',#9520);
#2794=VERTEX_POINT('',#9522);
#2795=VERTEX_POINT('',#9532);
#2796=VERTEX_POINT('',#9533);
#2797=VERTEX_POINT('',#9535);
#2798=VERTEX_POINT('',#9537);
#2799=VERTEX_POINT('',#9541);
#2800=VERTEX_POINT('',#9543);
#2801=VERTEX_POINT('',#9547);
#2802=VERTEX_POINT('',#9549);
#2803=VERTEX_POINT('',#9559);
#2804=VERTEX_POINT('',#9561);
#2805=VERTEX_POINT('',#9565);
#2806=VERTEX_POINT('',#9567);
#2807=VERTEX_POINT('',#9571);
#2808=VERTEX_POINT('',#9573);
#2809=VERTEX_POINT('',#9577);
#2810=VERTEX_POINT('',#9579);
#2811=VERTEX_POINT('',#9582);
#2812=VERTEX_POINT('',#9586);
#2813=VERTEX_POINT('',#9591);
#2814=VERTEX_POINT('',#9593);
#2815=VERTEX_POINT('',#9596);
#2816=VERTEX_POINT('',#9600);
#2817=VERTEX_POINT('',#9607);
#2818=VERTEX_POINT('',#9608);
#2819=VERTEX_POINT('',#9612);
#2820=VERTEX_POINT('',#9627);
#2821=VERTEX_POINT('',#9629);
#2822=VERTEX_POINT('',#9638);
#2823=VERTEX_POINT('',#9640);
#2824=VERTEX_POINT('',#9688);
#2825=VERTEX_POINT('',#9690);
#2826=VERTEX_POINT('',#9694);
#2827=VERTEX_POINT('',#9696);
#2828=VERTEX_POINT('',#9703);
#2829=VERTEX_POINT('',#9705);
#2830=VERTEX_POINT('',#9710);
#2831=VERTEX_POINT('',#9745);
#2832=VERTEX_POINT('',#9782);
#2833=VERTEX_POINT('',#9784);
#2834=VERTEX_POINT('',#9791);
#2835=VERTEX_POINT('',#9793);
#2836=VERTEX_POINT('',#9795);
#2837=VERTEX_POINT('',#9802);
#2838=VERTEX_POINT('',#9806);
#2839=VERTEX_POINT('',#9807);
#2840=VERTEX_POINT('',#9809);
#2841=VERTEX_POINT('',#10290);
#2842=VERTEX_POINT('',#10291);
#2843=VERTEX_POINT('',#10353);
#2844=VERTEX_POINT('',#10355);
#2845=VERTEX_POINT('',#10404);
#2846=VERTEX_POINT('',#10413);
#2847=VERTEX_POINT('',#10415);
#2848=VERTEX_POINT('',#10420);
#2849=VERTEX_POINT('',#10422);
#2850=VERTEX_POINT('',#10426);
#2851=VERTEX_POINT('',#10427);
#2852=VERTEX_POINT('',#10429);
#2853=VERTEX_POINT('',#10431);
#2854=VERTEX_POINT('',#10435);
#2855=VERTEX_POINT('',#10437);
#2856=VERTEX_POINT('',#10441);
#2857=VERTEX_POINT('',#10443);
#2858=VERTEX_POINT('',#10453);
#2859=VERTEX_POINT('',#10455);
#2860=VERTEX_POINT('',#10459);
#2861=VERTEX_POINT('',#10463);
#2862=VERTEX_POINT('',#10466);
#2863=VERTEX_POINT('',#10472);
#2864=VERTEX_POINT('',#10475);
#2865=VERTEX_POINT('',#10479);
#2866=VERTEX_POINT('',#10483);
#2867=VERTEX_POINT('',#10487);
#2868=VERTEX_POINT('',#10490);
#2869=VERTEX_POINT('',#10494);
#2870=VERTEX_POINT('',#10498);
#2871=VERTEX_POINT('',#10503);
#2872=VERTEX_POINT('',#10504);
#2873=VERTEX_POINT('',#10506);
#2874=VERTEX_POINT('',#10508);
#2875=VERTEX_POINT('',#10512);
#2876=VERTEX_POINT('',#10514);
#2877=VERTEX_POINT('',#10518);
#2878=VERTEX_POINT('',#10520);
#2879=VERTEX_POINT('',#10524);
#2880=VERTEX_POINT('',#10526);
#2881=VERTEX_POINT('',#10530);
#2882=VERTEX_POINT('',#10532);
#2883=VERTEX_POINT('',#10542);
#2884=VERTEX_POINT('',#10543);
#2885=VERTEX_POINT('',#10547);
#2886=VERTEX_POINT('',#10551);
#2887=VERTEX_POINT('',#10554);
#2888=VERTEX_POINT('',#10558);
#2889=VERTEX_POINT('',#10562);
#2890=VERTEX_POINT('',#10570);
#2891=VERTEX_POINT('',#10572);
#2892=VERTEX_POINT('',#10574);
#2893=VERTEX_POINT('',#10578);
#2894=VERTEX_POINT('',#10582);
#2895=VERTEX_POINT('',#10586);
#2896=VERTEX_POINT('',#10590);
#2897=VERTEX_POINT('',#10605);
#2898=VERTEX_POINT('',#10607);
#2899=VERTEX_POINT('',#10619);
#2900=VERTEX_POINT('',#10622);
#2901=VERTEX_POINT('',#10626);
#2902=VERTEX_POINT('',#10630);
#2903=VERTEX_POINT('',#10634);
#2904=VERTEX_POINT('',#10637);
#2905=VERTEX_POINT('',#10641);
#2906=VERTEX_POINT('',#10645);
#2907=VERTEX_POINT('',#10650);
#2908=VERTEX_POINT('',#10651);
#2909=VERTEX_POINT('',#10653);
#2910=VERTEX_POINT('',#10655);
#2911=VERTEX_POINT('',#10659);
#2912=VERTEX_POINT('',#10661);
#2913=VERTEX_POINT('',#10665);
#2914=VERTEX_POINT('',#10667);
#2915=VERTEX_POINT('',#10671);
#2916=VERTEX_POINT('',#10673);
#2917=VERTEX_POINT('',#10677);
#2918=VERTEX_POINT('',#10679);
#2919=VERTEX_POINT('',#10690);
#2920=VERTEX_POINT('',#10692);
#2921=VERTEX_POINT('',#10696);
#2922=VERTEX_POINT('',#10698);
#2923=VERTEX_POINT('',#10702);
#2924=VERTEX_POINT('',#10704);
#2925=VERTEX_POINT('',#10708);
#2926=VERTEX_POINT('',#10710);
#2927=VERTEX_POINT('',#10714);
#2928=VERTEX_POINT('',#10716);
#2929=VERTEX_POINT('',#10720);
#2930=VERTEX_POINT('',#10722);
#2931=VERTEX_POINT('',#10726);
#2932=VERTEX_POINT('',#10728);
#2933=VERTEX_POINT('',#10732);
#2934=VERTEX_POINT('',#10734);
#2935=VERTEX_POINT('',#10738);
#2936=VERTEX_POINT('',#10740);
#2937=VERTEX_POINT('',#10744);
#2938=VERTEX_POINT('',#10746);
#2939=VERTEX_POINT('',#10750);
#2940=VERTEX_POINT('',#10751);
#2941=VERTEX_POINT('',#10753);
#2942=VERTEX_POINT('',#10755);
#2943=VERTEX_POINT('',#10759);
#2944=VERTEX_POINT('',#10761);
#2945=VERTEX_POINT('',#10765);
#2946=VERTEX_POINT('',#10769);
#2947=VERTEX_POINT('',#10777);
#2948=VERTEX_POINT('',#10779);
#2949=VERTEX_POINT('',#10783);
#2950=VERTEX_POINT('',#10785);
#2951=VERTEX_POINT('',#10789);
#2952=VERTEX_POINT('',#10791);
#2953=VERTEX_POINT('',#10795);
#2954=VERTEX_POINT('',#10797);
#2955=VERTEX_POINT('',#10801);
#2956=VERTEX_POINT('',#10803);
#2957=VERTEX_POINT('',#10807);
#2958=VERTEX_POINT('',#10810);
#2959=VERTEX_POINT('',#10814);
#2960=VERTEX_POINT('',#10816);
#2961=VERTEX_POINT('',#10823);
#2962=VERTEX_POINT('',#10825);
#2963=VERTEX_POINT('',#10829);
#2964=VERTEX_POINT('',#10831);
#2965=VERTEX_POINT('',#10835);
#2966=VERTEX_POINT('',#10837);
#2967=VERTEX_POINT('',#10841);
#2968=VERTEX_POINT('',#10843);
#2969=VERTEX_POINT('',#10847);
#2970=VERTEX_POINT('',#10849);
#2971=VERTEX_POINT('',#10853);
#2972=VERTEX_POINT('',#10856);
#2973=VERTEX_POINT('',#10860);
#2974=VERTEX_POINT('',#10862);
#2975=VERTEX_POINT('',#10869);
#2976=VERTEX_POINT('',#10871);
#2977=VERTEX_POINT('',#10875);
#2978=VERTEX_POINT('',#10877);
#2979=VERTEX_POINT('',#10881);
#2980=VERTEX_POINT('',#10883);
#2981=VERTEX_POINT('',#10887);
#2982=VERTEX_POINT('',#10889);
#2983=VERTEX_POINT('',#10893);
#2984=VERTEX_POINT('',#10895);
#2985=VERTEX_POINT('',#10899);
#2986=VERTEX_POINT('',#10902);
#2987=VERTEX_POINT('',#10906);
#2988=VERTEX_POINT('',#10908);
#2989=VERTEX_POINT('',#10915);
#2990=VERTEX_POINT('',#10917);
#2991=VERTEX_POINT('',#10921);
#2992=VERTEX_POINT('',#10923);
#2993=VERTEX_POINT('',#10927);
#2994=VERTEX_POINT('',#10929);
#2995=VERTEX_POINT('',#10933);
#2996=VERTEX_POINT('',#10935);
#2997=VERTEX_POINT('',#10939);
#2998=VERTEX_POINT('',#10941);
#2999=VERTEX_POINT('',#10945);
#3000=VERTEX_POINT('',#10948);
#3001=VERTEX_POINT('',#10952);
#3002=VERTEX_POINT('',#10954);
#3003=VERTEX_POINT('',#10961);
#3004=VERTEX_POINT('',#10962);
#3005=VERTEX_POINT('',#10973);
#3006=VERTEX_POINT('',#11002);
#3007=VERTEX_POINT('',#11004);
#3008=VERTEX_POINT('',#11042);
#3009=VERTEX_POINT('',#11045);
#3010=VERTEX_POINT('',#11047);
#3011=VERTEX_POINT('',#11049);
#3012=VERTEX_POINT('',#11054);
#3013=VERTEX_POINT('',#11058);
#3014=VERTEX_POINT('',#11062);
#3015=VERTEX_POINT('',#11064);
#3016=VERTEX_POINT('',#11068);
#3017=VERTEX_POINT('',#11069);
#3018=VERTEX_POINT('',#11074);
#3019=VERTEX_POINT('',#11078);
#3020=VERTEX_POINT('',#11087);
#3021=VERTEX_POINT('',#11088);
#3022=VERTEX_POINT('',#11091);
#3023=VERTEX_POINT('',#11093);
#3024=VERTEX_POINT('',#11097);
#3025=VERTEX_POINT('',#11101);
#3026=VERTEX_POINT('',#11103);
#3027=VERTEX_POINT('',#11107);
#3028=VERTEX_POINT('',#11112);
#3029=VERTEX_POINT('',#11116);
#3030=VERTEX_POINT('',#11122);
#3031=VERTEX_POINT('',#11123);
#3032=VERTEX_POINT('',#11126);
#3033=VERTEX_POINT('',#11128);
#3034=VERTEX_POINT('',#11132);
#3035=VERTEX_POINT('',#11136);
#3036=VERTEX_POINT('',#11138);
#3037=VERTEX_POINT('',#11141);
#3038=VERTEX_POINT('',#11145);
#3039=VERTEX_POINT('',#11149);
#3040=VERTEX_POINT('',#11157);
#3041=VERTEX_POINT('',#11158);
#3042=VERTEX_POINT('',#11161);
#3043=VERTEX_POINT('',#11162);
#3044=VERTEX_POINT('',#11165);
#3045=VERTEX_POINT('',#11166);
#3046=VERTEX_POINT('',#11169);
#3047=VERTEX_POINT('',#11170);
#3048=VERTEX_POINT('',#11173);
#3049=VERTEX_POINT('',#11174);
#3050=VERTEX_POINT('',#11177);
#3051=VERTEX_POINT('',#11178);
#3052=VERTEX_POINT('',#11181);
#3053=VERTEX_POINT('',#11182);
#3054=VERTEX_POINT('',#11185);
#3055=VERTEX_POINT('',#11186);
#3056=VERTEX_POINT('',#11190);
#3057=VERTEX_POINT('',#11191);
#3058=VERTEX_POINT('',#11214);
#3059=VERTEX_POINT('',#11216);
#3060=VERTEX_POINT('',#11241);
#3061=VERTEX_POINT('',#11243);
#3062=VERTEX_POINT('',#11266);
#3063=VERTEX_POINT('',#11268);
#3064=VERTEX_POINT('',#11291);
#3065=VERTEX_POINT('',#11293);
#3066=VERTEX_POINT('',#11306);
#3067=VERTEX_POINT('',#11309);
#3068=VERTEX_POINT('',#11322);
#3069=VERTEX_POINT('',#11324);
#3070=VERTEX_POINT('',#11347);
#3071=VERTEX_POINT('',#11349);
#3072=VERTEX_POINT('',#11372);
#3073=VERTEX_POINT('',#11374);
#3074=VERTEX_POINT('',#11397);
#3075=VERTEX_POINT('',#11399);
#3076=VERTEX_POINT('',#11424);
#3077=VERTEX_POINT('',#11428);
#3078=VERTEX_POINT('',#11453);
#3079=VERTEX_POINT('',#11457);
#3080=VERTEX_POINT('',#11482);
#3081=VERTEX_POINT('',#11486);
#3082=VERTEX_POINT('',#11487);
#3083=VERTEX_POINT('',#11514);
#3084=VERTEX_POINT('',#11518);
#3085=VERTEX_POINT('',#11543);
#3086=VERTEX_POINT('',#11547);
#3087=VERTEX_POINT('',#11572);
#3088=VERTEX_POINT('',#11576);
#3089=VERTEX_POINT('',#11601);
#3090=VERTEX_POINT('',#11604);
#3091=VERTEX_POINT('',#11606);
#3092=VERTEX_POINT('',#11638);
#3093=VERTEX_POINT('',#11640);
#3094=VERTEX_POINT('',#11643);
#3095=VERTEX_POINT('',#11647);
#3096=VERTEX_POINT('',#11652);
#3097=VERTEX_POINT('',#11654);
#3098=VERTEX_POINT('',#11657);
#3099=VERTEX_POINT('',#11661);
#3100=VERTEX_POINT('',#11672);
#3101=VERTEX_POINT('',#11675);
#3102=VERTEX_POINT('',#11678);
#3103=VERTEX_POINT('',#11682);
#3104=VERTEX_POINT('',#11686);
#3105=VERTEX_POINT('',#11690);
#3106=VERTEX_POINT('',#11693);
#3107=VERTEX_POINT('',#11699);
#3108=VERTEX_POINT('',#11700);
#3109=VERTEX_POINT('',#11702);
#3110=VERTEX_POINT('',#11704);
#3111=VERTEX_POINT('',#11708);
#3112=VERTEX_POINT('',#11710);
#3113=VERTEX_POINT('',#11714);
#3114=VERTEX_POINT('',#11716);
#3115=VERTEX_POINT('',#11720);
#3116=VERTEX_POINT('',#11722);
#3117=VERTEX_POINT('',#11726);
#3118=VERTEX_POINT('',#11728);
#3119=VERTEX_POINT('',#11763);
#3120=VERTEX_POINT('',#11765);
#3121=VERTEX_POINT('',#11770);
#3122=VERTEX_POINT('',#11772);
#3123=VERTEX_POINT('',#11777);
#3124=VERTEX_POINT('',#11779);
#3125=VERTEX_POINT('',#11782);
#3126=VERTEX_POINT('',#11786);
#3127=VERTEX_POINT('',#11793);
#3128=VERTEX_POINT('',#11794);
#3129=VERTEX_POINT('',#11798);
#3130=VERTEX_POINT('',#11813);
#3131=VERTEX_POINT('',#11815);
#3132=VERTEX_POINT('',#11824);
#3133=VERTEX_POINT('',#11826);
#3134=VERTEX_POINT('',#11874);
#3135=VERTEX_POINT('',#11876);
#3136=VERTEX_POINT('',#11880);
#3137=VERTEX_POINT('',#11882);
#3138=VERTEX_POINT('',#11889);
#3139=VERTEX_POINT('',#11891);
#3140=VERTEX_POINT('',#11895);
#3141=VERTEX_POINT('',#11897);
#3142=VERTEX_POINT('',#11904);
#3143=VERTEX_POINT('',#11906);
#3144=VERTEX_POINT('',#11910);
#3145=VERTEX_POINT('',#11912);
#3146=VERTEX_POINT('',#11919);
#3147=VERTEX_POINT('',#11921);
#3148=VERTEX_POINT('',#11928);
#3149=VERTEX_POINT('',#11930);
#3150=VERTEX_POINT('',#11937);
#3151=VERTEX_POINT('',#11939);
#3152=VERTEX_POINT('',#11943);
#3153=VERTEX_POINT('',#11945);
#3154=VERTEX_POINT('',#11952);
#3155=VERTEX_POINT('',#11955);
#3156=VERTEX_POINT('',#11956);
#3157=VERTEX_POINT('',#11958);
#3158=VERTEX_POINT('',#11960);
#3159=VERTEX_POINT('',#11964);
#3160=VERTEX_POINT('',#11966);
#3161=VERTEX_POINT('',#11970);
#3162=VERTEX_POINT('',#11972);
#3163=VERTEX_POINT('',#11976);
#3164=VERTEX_POINT('',#11978);
#3165=VERTEX_POINT('',#11982);
#3166=VERTEX_POINT('',#11984);
#3167=VERTEX_POINT('',#11992);
#3168=VERTEX_POINT('',#11995);
#3169=VERTEX_POINT('',#12021);
#3170=VERTEX_POINT('',#12022);
#3171=VERTEX_POINT('',#12033);
#3172=VERTEX_POINT('',#12062);
#3173=VERTEX_POINT('',#12064);
#3174=VERTEX_POINT('',#12075);
#3175=VERTEX_POINT('',#12086);
#3176=VERTEX_POINT('',#12108);
#3177=VERTEX_POINT('',#12109);
#3178=VERTEX_POINT('',#12146);
#3179=VERTEX_POINT('',#12148);
#3180=VERTEX_POINT('',#12159);
#3181=VERTEX_POINT('',#12189);
#3182=VERTEX_POINT('',#12192);
#3183=VERTEX_POINT('',#12195);
#3184=VERTEX_POINT('',#12196);
#3185=VERTEX_POINT('',#12215);
#3186=VERTEX_POINT('',#12236);
#3187=VERTEX_POINT('',#12237);
#3188=VERTEX_POINT('',#12256);
#3189=VERTEX_POINT('',#12278);
#3190=VERTEX_POINT('',#12280);
#3191=VERTEX_POINT('',#12318);
#3192=VERTEX_POINT('',#12319);
#3193=VERTEX_POINT('',#12358);
#3194=VERTEX_POINT('',#12361);
#3195=VERTEX_POINT('',#12366);
#3196=VERTEX_POINT('',#12368);
#3197=VERTEX_POINT('',#12369);
#3198=VERTEX_POINT('',#12371);
#3199=VERTEX_POINT('',#12373);
#3200=VERTEX_POINT('',#12375);
#3201=VERTEX_POINT('',#12377);
#3202=VERTEX_POINT('',#12379);
#3203=VERTEX_POINT('',#12381);
#3204=VERTEX_POINT('',#12383);
#3205=VERTEX_POINT('',#12385);
#3206=VERTEX_POINT('',#12387);
#3207=VERTEX_POINT('',#12389);
#3208=VERTEX_POINT('',#12391);
#3209=VERTEX_POINT('',#12393);
#3210=VERTEX_POINT('',#12395);
#3211=VERTEX_POINT('',#12397);
#3212=VERTEX_POINT('',#12399);
#3213=VERTEX_POINT('',#12401);
#3214=VERTEX_POINT('',#12403);
#3215=VERTEX_POINT('',#12405);
#3216=VERTEX_POINT('',#12407);
#3217=VERTEX_POINT('',#12409);
#3218=VERTEX_POINT('',#12411);
#3219=VERTEX_POINT('',#12413);
#3220=VERTEX_POINT('',#12415);
#3221=VERTEX_POINT('',#12417);
#3222=VERTEX_POINT('',#12419);
#3223=VERTEX_POINT('',#12421);
#3224=VERTEX_POINT('',#12423);
#3225=VERTEX_POINT('',#12425);
#3226=VERTEX_POINT('',#12427);
#3227=VERTEX_POINT('',#12429);
#3228=VERTEX_POINT('',#12431);
#3229=VERTEX_POINT('',#12433);
#3230=VERTEX_POINT('',#12435);
#3231=VERTEX_POINT('',#12437);
#3232=VERTEX_POINT('',#12439);
#3233=VERTEX_POINT('',#12441);
#3234=VERTEX_POINT('',#12443);
#3235=VERTEX_POINT('',#12445);
#3236=VERTEX_POINT('',#12449);
#3237=VERTEX_POINT('',#12454);
#3238=VERTEX_POINT('',#12456);
#3239=VERTEX_POINT('',#12457);
#3240=VERTEX_POINT('',#12459);
#3241=VERTEX_POINT('',#12461);
#3242=VERTEX_POINT('',#12463);
#3243=VERTEX_POINT('',#12465);
#3244=VERTEX_POINT('',#12467);
#3245=VERTEX_POINT('',#12469);
#3246=VERTEX_POINT('',#12471);
#3247=VERTEX_POINT('',#12473);
#3248=VERTEX_POINT('',#12475);
#3249=VERTEX_POINT('',#12477);
#3250=VERTEX_POINT('',#12479);
#3251=VERTEX_POINT('',#12481);
#3252=VERTEX_POINT('',#12483);
#3253=VERTEX_POINT('',#12485);
#3254=VERTEX_POINT('',#12487);
#3255=VERTEX_POINT('',#12489);
#3256=VERTEX_POINT('',#12491);
#3257=VERTEX_POINT('',#12493);
#3258=VERTEX_POINT('',#12495);
#3259=VERTEX_POINT('',#12497);
#3260=VERTEX_POINT('',#12499);
#3261=VERTEX_POINT('',#12501);
#3262=VERTEX_POINT('',#12503);
#3263=VERTEX_POINT('',#12505);
#3264=VERTEX_POINT('',#12507);
#3265=VERTEX_POINT('',#12509);
#3266=VERTEX_POINT('',#12511);
#3267=VERTEX_POINT('',#12513);
#3268=VERTEX_POINT('',#12515);
#3269=VERTEX_POINT('',#12517);
#3270=VERTEX_POINT('',#12519);
#3271=VERTEX_POINT('',#12521);
#3272=VERTEX_POINT('',#12523);
#3273=VERTEX_POINT('',#12525);
#3274=VERTEX_POINT('',#12527);
#3275=VERTEX_POINT('',#12529);
#3276=VERTEX_POINT('',#12531);
#3277=VERTEX_POINT('',#12533);
#3278=VERTEX_POINT('',#12537);
#3279=VERTEX_POINT('',#12623);
#3280=VERTEX_POINT('',#12624);
#3281=VERTEX_POINT('',#12626);
#3282=VERTEX_POINT('',#12628);
#3283=VERTEX_POINT('',#12632);
#3284=VERTEX_POINT('',#12634);
#3285=VERTEX_POINT('',#12638);
#3286=VERTEX_POINT('',#12640);
#3287=VERTEX_POINT('',#12644);
#3288=VERTEX_POINT('',#12646);
#3289=VERTEX_POINT('',#12650);
#3290=VERTEX_POINT('',#12652);
#3291=VERTEX_POINT('',#12661);
#3292=VERTEX_POINT('',#12664);
#3293=VERTEX_POINT('',#12667);
#3294=VERTEX_POINT('',#12671);
#3295=VERTEX_POINT('',#12675);
#3296=VERTEX_POINT('',#12679);
#3297=VERTEX_POINT('',#12682);
#3298=EDGE_CURVE('',#2769,#2769,#2405,.T.);
#3299=EDGE_CURVE('',#2769,#2770,#1707,.T.);
#3300=EDGE_CURVE('',#2770,#2770,#2406,.T.);
#3301=EDGE_CURVE('',#2771,#2771,#2407,.T.);
#3302=EDGE_CURVE('',#2771,#2772,#1708,.T.);
#3303=EDGE_CURVE('',#2772,#2772,#2408,.T.);
#3304=EDGE_CURVE('',#2773,#2773,#2409,.T.);
#3305=EDGE_CURVE('',#2773,#2774,#1709,.T.);
#3306=EDGE_CURVE('',#2774,#2774,#2410,.T.);
#3307=EDGE_CURVE('',#2775,#2775,#2411,.T.);
#3308=EDGE_CURVE('',#2775,#2776,#1710,.T.);
#3309=EDGE_CURVE('',#2776,#2776,#2412,.T.);
#3310=EDGE_CURVE('',#2777,#2777,#2413,.T.);
#3311=EDGE_CURVE('',#2777,#2778,#1711,.T.);
#3312=EDGE_CURVE('',#2778,#2778,#2414,.T.);
#3313=EDGE_CURVE('',#2779,#2780,#1712,.T.);
#3314=EDGE_CURVE('',#2780,#2781,#1713,.T.);
#3315=EDGE_CURVE('',#2782,#2781,#1714,.T.);
#3316=EDGE_CURVE('',#2779,#2782,#1715,.T.);
#3317=EDGE_CURVE('',#2783,#2779,#1716,.T.);
#3318=EDGE_CURVE('',#2784,#2782,#1717,.T.);
#3319=EDGE_CURVE('',#2783,#2784,#1718,.T.);
#3320=EDGE_CURVE('',#2785,#2783,#1719,.T.);
#3321=EDGE_CURVE('',#2786,#2784,#1720,.T.);
#3322=EDGE_CURVE('',#2785,#2786,#1721,.T.);
#3323=EDGE_CURVE('',#2780,#2785,#1722,.T.);
#3324=EDGE_CURVE('',#2781,#2786,#1723,.T.);
#3325=EDGE_CURVE('',#2787,#2788,#1724,.T.);
#3326=EDGE_CURVE('',#2788,#2789,#1725,.T.);
#3327=EDGE_CURVE('',#2790,#2789,#1726,.T.);
#3328=EDGE_CURVE('',#2787,#2790,#1727,.T.);
#3329=EDGE_CURVE('',#2791,#2787,#1728,.T.);
#3330=EDGE_CURVE('',#2792,#2790,#1729,.T.);
#3331=EDGE_CURVE('',#2791,#2792,#1730,.T.);
#3332=EDGE_CURVE('',#2793,#2791,#1731,.T.);
#3333=EDGE_CURVE('',#2794,#2792,#1732,.T.);
#3334=EDGE_CURVE('',#2793,#2794,#1733,.T.);
#3335=EDGE_CURVE('',#2788,#2793,#1734,.T.);
#3336=EDGE_CURVE('',#2789,#2794,#1735,.T.);
#3337=EDGE_CURVE('',#2795,#2796,#1736,.T.);
#3338=EDGE_CURVE('',#2796,#2797,#1737,.T.);
#3339=EDGE_CURVE('',#2798,#2797,#1738,.T.);
#3340=EDGE_CURVE('',#2795,#2798,#1739,.T.);
#3341=EDGE_CURVE('',#2799,#2795,#1740,.T.);
#3342=EDGE_CURVE('',#2800,#2798,#1741,.T.);
#3343=EDGE_CURVE('',#2799,#2800,#1742,.T.);
#3344=EDGE_CURVE('',#2801,#2799,#1743,.T.);
#3345=EDGE_CURVE('',#2802,#2800,#1744,.T.);
#3346=EDGE_CURVE('',#2801,#2802,#1745,.T.);
#3347=EDGE_CURVE('',#2796,#2801,#1746,.T.);
#3348=EDGE_CURVE('',#2797,#2802,#1747,.T.);
#3349=EDGE_CURVE('',#2803,#2803,#2415,.T.);
#3350=EDGE_CURVE('',#2803,#2804,#1748,.T.);
#3351=EDGE_CURVE('',#2804,#2804,#2416,.T.);
#3352=EDGE_CURVE('',#2805,#2805,#2417,.T.);
#3353=EDGE_CURVE('',#2805,#2806,#1749,.T.);
#3354=EDGE_CURVE('',#2806,#2806,#2418,.T.);
#3355=EDGE_CURVE('',#2807,#2807,#2419,.T.);
#3356=EDGE_CURVE('',#2807,#2808,#1750,.T.);
#3357=EDGE_CURVE('',#2808,#2808,#2420,.T.);
#3358=EDGE_CURVE('',#2809,#2809,#2421,.T.);
#3359=EDGE_CURVE('',#2810,#2810,#2422,.T.);
#3360=EDGE_CURVE('',#2809,#2811,#1751,.T.);
#3361=EDGE_CURVE('',#2811,#2811,#2423,.T.);
#3362=EDGE_CURVE('',#2812,#2812,#2424,.T.);
#3363=EDGE_CURVE('',#2812,#2810,#1752,.T.);
#3364=EDGE_CURVE('',#2813,#2813,#2425,.T.);
#3365=EDGE_CURVE('',#2814,#2814,#2426,.T.);
#3366=EDGE_CURVE('',#2813,#2815,#1753,.T.);
#3367=EDGE_CURVE('',#2815,#2815,#2427,.T.);
#3368=EDGE_CURVE('',#2816,#2816,#2428,.T.);
#3369=EDGE_CURVE('',#2816,#2814,#1754,.T.);
#3370=EDGE_CURVE('',#2817,#2818,#1755,.T.);
#3371=EDGE_CURVE('',#2817,#2818,#2429,.T.);
#3372=EDGE_CURVE('',#2819,#2817,#317,.T.);
#3373=EDGE_CURVE('',#2820,#2819,#2430,.T.);
#3374=EDGE_CURVE('',#2821,#2820,#318,.T.);
#3375=EDGE_CURVE('',#2821,#2822,#1756,.T.);
#3376=EDGE_CURVE('',#2823,#2822,#319,.T.);
#3377=EDGE_CURVE('',#2822,#2823,#320,.T.);
#3378=EDGE_CURVE('',#2818,#2821,#321,.T.);
#3379=EDGE_CURVE('',#2820,#2819,#1757,.T.);
#3380=EDGE_CURVE('',#2824,#2824,#2431,.T.);
#3381=EDGE_CURVE('',#2824,#2825,#1758,.T.);
#3382=EDGE_CURVE('',#2825,#2825,#2432,.T.);
#3383=EDGE_CURVE('',#2826,#2826,#2433,.T.);
#3384=EDGE_CURVE('',#2826,#2827,#1759,.T.);
#3385=EDGE_CURVE('',#2827,#2827,#2434,.T.);
#3386=EDGE_CURVE('',#2828,#2828,#2435,.T.);
#3387=EDGE_CURVE('',#2828,#2829,#1760,.T.);
#3388=EDGE_CURVE('',#2829,#2829,#2436,.T.);
#3389=EDGE_CURVE('',#2830,#2830,#322,.T.);
#3390=EDGE_CURVE('',#2830,#2831,#1761,.T.);
#3391=EDGE_CURVE('',#2831,#2831,#323,.T.);
#3392=EDGE_CURVE('',#2832,#2832,#2437,.T.);
#3393=EDGE_CURVE('',#2832,#2833,#1762,.T.);
#3394=EDGE_CURVE('',#2833,#2833,#2438,.T.);
#3395=EDGE_CURVE('',#2834,#2834,#2439,.T.);
#3396=EDGE_CURVE('',#2834,#2835,#1763,.T.);
#3397=EDGE_CURVE('',#2836,#2835,#316,.T.);
#3398=EDGE_CURVE('',#2836,#2835,#2440,.T.);
#3399=EDGE_CURVE('',#2835,#2836,#1764,.T.);
#3400=EDGE_CURVE('',#2836,#2837,#2441,.T.);
#3401=EDGE_CURVE('',#2837,#2835,#2442,.T.);
#3402=EDGE_CURVE('',#2838,#2839,#2443,.T.);
#3403=EDGE_CURVE('',#2840,#2839,#324,.T.);
#3404=EDGE_CURVE('',#2838,#2840,#325,.T.);
#3405=EDGE_CURVE('',#2837,#2838,#1765,.T.);
#3406=EDGE_CURVE('',#2839,#2838,#1766,.T.);
#3407=EDGE_CURVE('',#2838,#2839,#2444,.T.);
#3408=EDGE_CURVE('',#2841,#2842,#326,.T.);
#3409=EDGE_CURVE('',#2842,#2843,#2445,.T.);
#3410=EDGE_CURVE('',#2843,#2844,#327,.T.);
#3411=EDGE_CURVE('',#2844,#2840,#328,.T.);
#3412=EDGE_CURVE('',#2843,#2841,#2446,.T.);
#3413=EDGE_CURVE('',#2842,#2841,#2447,.T.);
#3414=EDGE_CURVE('',#2841,#2845,#1767,.T.);
#3415=EDGE_CURVE('',#2845,#2845,#2448,.T.);
#3416=EDGE_CURVE('',#2842,#2841,#1768,.T.);
#3417=EDGE_CURVE('',#2846,#2846,#2449,.T.);
#3418=EDGE_CURVE('',#2846,#2847,#1769,.T.);
#3419=EDGE_CURVE('',#2847,#2847,#2450,.T.);
#3420=EDGE_CURVE('',#2848,#2848,#2451,.T.);
#3421=EDGE_CURVE('',#2848,#2849,#1770,.T.);
#3422=EDGE_CURVE('',#2849,#2849,#2452,.T.);
#3423=EDGE_CURVE('',#2850,#2851,#1771,.T.);
#3424=EDGE_CURVE('',#2851,#2852,#1772,.T.);
#3425=EDGE_CURVE('',#2853,#2852,#1773,.T.);
#3426=EDGE_CURVE('',#2850,#2853,#1774,.T.);
#3427=EDGE_CURVE('',#2854,#2850,#1775,.T.);
#3428=EDGE_CURVE('',#2855,#2853,#1776,.T.);
#3429=EDGE_CURVE('',#2854,#2855,#1777,.T.);
#3430=EDGE_CURVE('',#2856,#2854,#1778,.T.);
#3431=EDGE_CURVE('',#2857,#2855,#1779,.T.);
#3432=EDGE_CURVE('',#2856,#2857,#1780,.T.);
#3433=EDGE_CURVE('',#2851,#2856,#1781,.T.);
#3434=EDGE_CURVE('',#2852,#2857,#1782,.T.);
#3435=EDGE_CURVE('',#2858,#2858,#2453,.T.);
#3436=EDGE_CURVE('',#2858,#2859,#1783,.T.);
#3437=EDGE_CURVE('',#2859,#2859,#2454,.T.);
#3438=EDGE_CURVE('',#2859,#2860,#1784,.T.);
#3439=EDGE_CURVE('',#2860,#2860,#2455,.T.);
#3440=EDGE_CURVE('',#2861,#2861,#2456,.T.);
#3441=EDGE_CURVE('',#2861,#2862,#1785,.T.);
#3442=EDGE_CURVE('',#2862,#2862,#2457,.T.);
#3443=EDGE_CURVE('',#2863,#2863,#2458,.T.);
#3444=EDGE_CURVE('',#2864,#2864,#2459,.T.);
#3445=EDGE_CURVE('',#2864,#2863,#1786,.T.);
#3446=EDGE_CURVE('',#2865,#2865,#2460,.T.);
#3447=EDGE_CURVE('',#2865,#2864,#1787,.T.);
#3448=EDGE_CURVE('',#2866,#2866,#2461,.T.);
#3449=EDGE_CURVE('',#2866,#2865,#1788,.T.);
#3450=EDGE_CURVE('',#2867,#2867,#2462,.T.);
#3451=EDGE_CURVE('',#2868,#2868,#2463,.F.);
#3452=EDGE_CURVE('',#2868,#2867,#1789,.T.);
#3453=EDGE_CURVE('',#2869,#2869,#2464,.F.);
#3454=EDGE_CURVE('',#2869,#2868,#1790,.T.);
#3455=EDGE_CURVE('',#2870,#2870,#2465,.T.);
#3456=EDGE_CURVE('',#2870,#2869,#1791,.T.);
#3457=EDGE_CURVE('',#2871,#2872,#1792,.T.);
#3458=EDGE_CURVE('',#2872,#2873,#1793,.T.);
#3459=EDGE_CURVE('',#2873,#2874,#1794,.T.);
#3460=EDGE_CURVE('',#2871,#2874,#1795,.T.);
#3461=EDGE_CURVE('',#2872,#2875,#1796,.T.);
#3462=EDGE_CURVE('',#2875,#2876,#1797,.T.);
#3463=EDGE_CURVE('',#2876,#2873,#1798,.T.);
#3464=EDGE_CURVE('',#2875,#2877,#1799,.T.);
#3465=EDGE_CURVE('',#2877,#2878,#1800,.T.);
#3466=EDGE_CURVE('',#2878,#2876,#1801,.T.);
#3467=EDGE_CURVE('',#2877,#2879,#1802,.T.);
#3468=EDGE_CURVE('',#2879,#2880,#1803,.T.);
#3469=EDGE_CURVE('',#2880,#2878,#1804,.T.);
#3470=EDGE_CURVE('',#2879,#2881,#1805,.T.);
#3471=EDGE_CURVE('',#2881,#2882,#1806,.T.);
#3472=EDGE_CURVE('',#2882,#2880,#1807,.T.);
#3473=EDGE_CURVE('',#2881,#2871,#1808,.T.);
#3474=EDGE_CURVE('',#2874,#2882,#1809,.T.);
#3475=EDGE_CURVE('',#2883,#2884,#273,.T.);
#3476=EDGE_CURVE('',#2885,#2883,#274,.T.);
#3477=EDGE_CURVE('',#2885,#2886,#1810,.T.);
#3478=EDGE_CURVE('',#2886,#2886,#2466,.T.);
#3479=EDGE_CURVE('',#2887,#2885,#275,.T.);
#3480=EDGE_CURVE('',#2888,#2887,#276,.T.);
#3481=EDGE_CURVE('',#2889,#2888,#277,.T.);
#3482=EDGE_CURVE('',#2884,#2889,#278,.T.);
#3483=EDGE_CURVE('',#2890,#2890,#2467,.T.);
#3484=EDGE_CURVE('',#2890,#2891,#1811,.T.);
#3485=EDGE_CURVE('',#2892,#2891,#279,.T.);
#3486=EDGE_CURVE('',#2893,#2892,#280,.T.);
#3487=EDGE_CURVE('',#2894,#2893,#281,.T.);
#3488=EDGE_CURVE('',#2895,#2894,#282,.T.);
#3489=EDGE_CURVE('',#2896,#2895,#283,.T.);
#3490=EDGE_CURVE('',#2891,#2896,#284,.T.);
#3491=EDGE_CURVE('',#2887,#2896,#1812,.T.);
#3492=EDGE_CURVE('',#2888,#2895,#1813,.T.);
#3493=EDGE_CURVE('',#2885,#2891,#1814,.T.);
#3494=EDGE_CURVE('',#2883,#2892,#1815,.T.);
#3495=EDGE_CURVE('',#2897,#2897,#2468,.F.);
#3496=EDGE_CURVE('',#2897,#2898,#1816,.T.);
#3497=EDGE_CURVE('',#2898,#2898,#2469,.F.);
#3498=EDGE_CURVE('',#2884,#2893,#1817,.T.);
#3499=EDGE_CURVE('',#2889,#2894,#1818,.T.);
#3500=EDGE_CURVE('',#2899,#2899,#2470,.T.);
#3501=EDGE_CURVE('',#2900,#2900,#2471,.T.);
#3502=EDGE_CURVE('',#2900,#2899,#1819,.T.);
#3503=EDGE_CURVE('',#2901,#2901,#2472,.T.);
#3504=EDGE_CURVE('',#2901,#2900,#1820,.T.);
#3505=EDGE_CURVE('',#2902,#2902,#2473,.T.);
#3506=EDGE_CURVE('',#2902,#2901,#1821,.T.);
#3507=EDGE_CURVE('',#2903,#2903,#2474,.T.);
#3508=EDGE_CURVE('',#2904,#2904,#2475,.F.);
#3509=EDGE_CURVE('',#2904,#2903,#1822,.T.);
#3510=EDGE_CURVE('',#2905,#2905,#2476,.F.);
#3511=EDGE_CURVE('',#2905,#2904,#1823,.T.);
#3512=EDGE_CURVE('',#2906,#2906,#2477,.T.);
#3513=EDGE_CURVE('',#2906,#2905,#1824,.T.);
#3514=EDGE_CURVE('',#2907,#2908,#1825,.T.);
#3515=EDGE_CURVE('',#2908,#2909,#1826,.T.);
#3516=EDGE_CURVE('',#2909,#2910,#1827,.T.);
#3517=EDGE_CURVE('',#2907,#2910,#1828,.T.);
#3518=EDGE_CURVE('',#2908,#2911,#1829,.T.);
#3519=EDGE_CURVE('',#2911,#2912,#1830,.T.);
#3520=EDGE_CURVE('',#2912,#2909,#1831,.T.);
#3521=EDGE_CURVE('',#2911,#2913,#1832,.T.);
#3522=EDGE_CURVE('',#2913,#2914,#1833,.T.);
#3523=EDGE_CURVE('',#2914,#2912,#1834,.T.);
#3524=EDGE_CURVE('',#2913,#2915,#1835,.T.);
#3525=EDGE_CURVE('',#2915,#2916,#1836,.T.);
#3526=EDGE_CURVE('',#2916,#2914,#1837,.T.);
#3527=EDGE_CURVE('',#2915,#2917,#1838,.T.);
#3528=EDGE_CURVE('',#2917,#2918,#1839,.T.);
#3529=EDGE_CURVE('',#2918,#2916,#1840,.T.);
#3530=EDGE_CURVE('',#2917,#2907,#1841,.T.);
#3531=EDGE_CURVE('',#2910,#2918,#1842,.T.);
#3532=EDGE_CURVE('',#2919,#2919,#2478,.T.);
#3533=EDGE_CURVE('',#2919,#2920,#1843,.T.);
#3534=EDGE_CURVE('',#2920,#2920,#2479,.T.);
#3535=EDGE_CURVE('',#2921,#2921,#2480,.T.);
#3536=EDGE_CURVE('',#2921,#2922,#1844,.T.);
#3537=EDGE_CURVE('',#2922,#2922,#2481,.T.);
#3538=EDGE_CURVE('',#2923,#2923,#2482,.T.);
#3539=EDGE_CURVE('',#2923,#2924,#1845,.T.);
#3540=EDGE_CURVE('',#2924,#2924,#2483,.T.);
#3541=EDGE_CURVE('',#2925,#2925,#2484,.T.);
#3542=EDGE_CURVE('',#2925,#2926,#1846,.T.);
#3543=EDGE_CURVE('',#2926,#2926,#2485,.T.);
#3544=EDGE_CURVE('',#2927,#2927,#2486,.T.);
#3545=EDGE_CURVE('',#2927,#2928,#1847,.T.);
#3546=EDGE_CURVE('',#2928,#2928,#2487,.T.);
#3547=EDGE_CURVE('',#2929,#2929,#2488,.T.);
#3548=EDGE_CURVE('',#2929,#2930,#1848,.T.);
#3549=EDGE_CURVE('',#2930,#2930,#2489,.T.);
#3550=EDGE_CURVE('',#2931,#2931,#2490,.T.);
#3551=EDGE_CURVE('',#2931,#2932,#1849,.T.);
#3552=EDGE_CURVE('',#2932,#2932,#2491,.T.);
#3553=EDGE_CURVE('',#2933,#2933,#2492,.T.);
#3554=EDGE_CURVE('',#2933,#2934,#1850,.T.);
#3555=EDGE_CURVE('',#2934,#2934,#2493,.T.);
#3556=EDGE_CURVE('',#2935,#2935,#2494,.T.);
#3557=EDGE_CURVE('',#2935,#2936,#1851,.T.);
#3558=EDGE_CURVE('',#2936,#2936,#2495,.T.);
#3559=EDGE_CURVE('',#2937,#2937,#2496,.T.);
#3560=EDGE_CURVE('',#2937,#2938,#1852,.T.);
#3561=EDGE_CURVE('',#2938,#2938,#2497,.T.);
#3562=EDGE_CURVE('',#2939,#2940,#1853,.T.);
#3563=EDGE_CURVE('',#2941,#2939,#2498,.T.);
#3564=EDGE_CURVE('',#2942,#2941,#1854,.T.);
#3565=EDGE_CURVE('',#2942,#2940,#2499,.T.);
#3566=EDGE_CURVE('',#2940,#2943,#1855,.T.);
#3567=EDGE_CURVE('',#2944,#2943,#1856,.T.);
#3568=EDGE_CURVE('',#2939,#2944,#1857,.T.);
#3569=EDGE_CURVE('',#2945,#2942,#1858,.T.);
#3570=EDGE_CURVE('',#2943,#2945,#2500,.T.);
#3571=EDGE_CURVE('',#2946,#2941,#1859,.T.);
#3572=EDGE_CURVE('',#2945,#2946,#1860,.T.);
#3573=EDGE_CURVE('',#2944,#2946,#2501,.T.);
#3574=EDGE_CURVE('',#2947,#2947,#2502,.T.);
#3575=EDGE_CURVE('',#2947,#2948,#1861,.T.);
#3576=EDGE_CURVE('',#2948,#2948,#2503,.T.);
#3577=EDGE_CURVE('',#2949,#2949,#2504,.T.);
#3578=EDGE_CURVE('',#2949,#2950,#1862,.T.);
#3579=EDGE_CURVE('',#2950,#2950,#2505,.T.);
#3580=EDGE_CURVE('',#2951,#2951,#2506,.T.);
#3581=EDGE_CURVE('',#2951,#2952,#1863,.T.);
#3582=EDGE_CURVE('',#2952,#2952,#2507,.T.);
#3583=EDGE_CURVE('',#2953,#2953,#2508,.T.);
#3584=EDGE_CURVE('',#2953,#2954,#1864,.T.);
#3585=EDGE_CURVE('',#2954,#2954,#2509,.T.);
#3586=EDGE_CURVE('',#2955,#2955,#2510,.T.);
#3587=EDGE_CURVE('',#2955,#2956,#1865,.T.);
#3588=EDGE_CURVE('',#2956,#2956,#2511,.T.);
#3589=EDGE_CURVE('',#2957,#2957,#2512,.T.);
#3590=EDGE_CURVE('',#2957,#2958,#1866,.T.);
#3591=EDGE_CURVE('',#2958,#2958,#2513,.T.);
#3592=EDGE_CURVE('',#2959,#2959,#2514,.T.);
#3593=EDGE_CURVE('',#2959,#2960,#1867,.T.);
#3594=EDGE_CURVE('',#2960,#2960,#2515,.T.);
#3595=EDGE_CURVE('',#2961,#2961,#2516,.T.);
#3596=EDGE_CURVE('',#2961,#2962,#1868,.T.);
#3597=EDGE_CURVE('',#2962,#2962,#2517,.T.);
#3598=EDGE_CURVE('',#2963,#2963,#2518,.T.);
#3599=EDGE_CURVE('',#2963,#2964,#1869,.T.);
#3600=EDGE_CURVE('',#2964,#2964,#2519,.T.);
#3601=EDGE_CURVE('',#2965,#2965,#2520,.T.);
#3602=EDGE_CURVE('',#2965,#2966,#1870,.T.);
#3603=EDGE_CURVE('',#2966,#2966,#2521,.T.);
#3604=EDGE_CURVE('',#2967,#2967,#2522,.T.);
#3605=EDGE_CURVE('',#2967,#2968,#1871,.T.);
#3606=EDGE_CURVE('',#2968,#2968,#2523,.T.);
#3607=EDGE_CURVE('',#2969,#2969,#2524,.T.);
#3608=EDGE_CURVE('',#2969,#2970,#1872,.T.);
#3609=EDGE_CURVE('',#2970,#2970,#2525,.T.);
#3610=EDGE_CURVE('',#2971,#2971,#2526,.T.);
#3611=EDGE_CURVE('',#2972,#2972,#2527,.T.);
#3612=EDGE_CURVE('',#2972,#2971,#1873,.T.);
#3613=EDGE_CURVE('',#2973,#2973,#2528,.T.);
#3614=EDGE_CURVE('',#2973,#2974,#1874,.T.);
#3615=EDGE_CURVE('',#2974,#2974,#2529,.T.);
#3616=EDGE_CURVE('',#2975,#2975,#2530,.T.);
#3617=EDGE_CURVE('',#2975,#2976,#1875,.T.);
#3618=EDGE_CURVE('',#2976,#2976,#2531,.T.);
#3619=EDGE_CURVE('',#2977,#2977,#2532,.T.);
#3620=EDGE_CURVE('',#2977,#2978,#1876,.T.);
#3621=EDGE_CURVE('',#2978,#2978,#2533,.T.);
#3622=EDGE_CURVE('',#2979,#2979,#2534,.T.);
#3623=EDGE_CURVE('',#2979,#2980,#1877,.T.);
#3624=EDGE_CURVE('',#2980,#2980,#2535,.T.);
#3625=EDGE_CURVE('',#2981,#2981,#2536,.T.);
#3626=EDGE_CURVE('',#2981,#2982,#1878,.T.);
#3627=EDGE_CURVE('',#2982,#2982,#2537,.T.);
#3628=EDGE_CURVE('',#2983,#2983,#2538,.T.);
#3629=EDGE_CURVE('',#2983,#2984,#1879,.T.);
#3630=EDGE_CURVE('',#2984,#2984,#2539,.T.);
#3631=EDGE_CURVE('',#2985,#2985,#2540,.T.);
#3632=EDGE_CURVE('',#2985,#2986,#1880,.T.);
#3633=EDGE_CURVE('',#2986,#2986,#2541,.T.);
#3634=EDGE_CURVE('',#2987,#2987,#2542,.T.);
#3635=EDGE_CURVE('',#2987,#2988,#1881,.T.);
#3636=EDGE_CURVE('',#2988,#2988,#2543,.T.);
#3637=EDGE_CURVE('',#2989,#2989,#2544,.T.);
#3638=EDGE_CURVE('',#2989,#2990,#1882,.T.);
#3639=EDGE_CURVE('',#2990,#2990,#2545,.T.);
#3640=EDGE_CURVE('',#2991,#2991,#2546,.T.);
#3641=EDGE_CURVE('',#2991,#2992,#1883,.T.);
#3642=EDGE_CURVE('',#2992,#2992,#2547,.T.);
#3643=EDGE_CURVE('',#2993,#2993,#2548,.T.);
#3644=EDGE_CURVE('',#2993,#2994,#1884,.T.);
#3645=EDGE_CURVE('',#2994,#2994,#2549,.T.);
#3646=EDGE_CURVE('',#2995,#2995,#2550,.T.);
#3647=EDGE_CURVE('',#2995,#2996,#1885,.T.);
#3648=EDGE_CURVE('',#2996,#2996,#2551,.T.);
#3649=EDGE_CURVE('',#2997,#2997,#2552,.T.);
#3650=EDGE_CURVE('',#2997,#2998,#1886,.T.);
#3651=EDGE_CURVE('',#2998,#2998,#2553,.T.);
#3652=EDGE_CURVE('',#2999,#2999,#2554,.T.);
#3653=EDGE_CURVE('',#3000,#3000,#2555,.T.);
#3654=EDGE_CURVE('',#3000,#2999,#1887,.T.);
#3655=EDGE_CURVE('',#3001,#3001,#2556,.T.);
#3656=EDGE_CURVE('',#3001,#3002,#1888,.T.);
#3657=EDGE_CURVE('',#3002,#3002,#2557,.T.);
#3658=EDGE_CURVE('',#3003,#3004,#329,.T.);
#3659=EDGE_CURVE('',#3005,#3003,#330,.T.);
#3660=EDGE_CURVE('',#3004,#3005,#331,.T.);
#3661=EDGE_CURVE('',#3004,#3006,#1889,.T.);
#3662=EDGE_CURVE('',#3007,#3006,#332,.T.);
#3663=EDGE_CURVE('',#3006,#3007,#333,.T.);
#3664=EDGE_CURVE('',#3008,#3008,#2558,.T.);
#3665=EDGE_CURVE('',#3008,#3004,#1890,.T.);
#3666=EDGE_CURVE('',#3005,#3009,#1891,.T.);
#3667=EDGE_CURVE('',#3010,#3009,#2559,.T.);
#3668=EDGE_CURVE('',#3011,#3010,#2560,.T.);
#3669=EDGE_CURVE('',#3009,#3011,#2561,.T.);
#3670=EDGE_CURVE('',#3011,#3012,#1892,.T.);
#3671=EDGE_CURVE('',#3012,#3009,#1893,.T.);
#3672=EDGE_CURVE('',#3010,#3013,#1894,.T.);
#3673=EDGE_CURVE('',#3013,#3011,#1895,.T.);
#3674=EDGE_CURVE('',#3009,#3014,#1896,.T.);
#3675=EDGE_CURVE('',#3014,#3015,#1897,.T.);
#3676=EDGE_CURVE('',#3015,#3010,#1898,.T.);
#3677=EDGE_CURVE('',#3016,#3017,#1899,.T.);
#3678=EDGE_CURVE('',#3017,#3012,#1900,.T.);
#3679=EDGE_CURVE('',#3016,#3013,#1901,.T.);
#3680=EDGE_CURVE('',#3018,#3016,#1902,.T.);
#3681=EDGE_CURVE('',#3018,#3015,#1903,.T.);
#3682=EDGE_CURVE('',#3019,#3018,#1904,.T.);
#3683=EDGE_CURVE('',#3019,#3014,#1905,.T.);
#3684=EDGE_CURVE('',#3017,#3019,#1906,.T.);
#3685=EDGE_CURVE('',#3020,#3021,#2562,.T.);
#3686=EDGE_CURVE('',#3021,#3020,#2563,.T.);
#3687=EDGE_CURVE('',#3021,#3022,#2564,.T.);
#3688=EDGE_CURVE('',#3023,#3022,#2565,.T.);
#3689=EDGE_CURVE('',#3022,#3023,#2566,.T.);
#3690=EDGE_CURVE('',#3023,#3024,#1907,.T.);
#3691=EDGE_CURVE('',#3024,#3024,#2567,.T.);
#3692=EDGE_CURVE('',#3025,#3025,#2568,.T.);
#3693=EDGE_CURVE('',#3025,#3026,#1908,.T.);
#3694=EDGE_CURVE('',#3026,#3026,#2569,.T.);
#3695=EDGE_CURVE('',#3026,#3027,#1909,.T.);
#3696=EDGE_CURVE('',#3027,#3027,#2570,.T.);
#3697=EDGE_CURVE('',#3028,#3028,#2571,.T.);
#3698=EDGE_CURVE('',#3028,#3020,#1910,.T.);
#3699=EDGE_CURVE('',#3029,#3029,#2572,.T.);
#3700=EDGE_CURVE('',#3029,#3025,#1911,.T.);
#3701=EDGE_CURVE('',#3030,#3031,#2573,.T.);
#3702=EDGE_CURVE('',#3031,#3030,#2574,.T.);
#3703=EDGE_CURVE('',#3031,#3032,#2575,.T.);
#3704=EDGE_CURVE('',#3033,#3032,#2576,.T.);
#3705=EDGE_CURVE('',#3032,#3033,#2577,.T.);
#3706=EDGE_CURVE('',#3034,#3034,#2578,.T.);
#3707=EDGE_CURVE('',#3034,#3033,#1912,.T.);
#3708=EDGE_CURVE('',#3035,#3035,#2579,.T.);
#3709=EDGE_CURVE('',#3036,#3036,#2580,.T.);
#3710=EDGE_CURVE('',#3037,#3037,#2581,.T.);
#3711=EDGE_CURVE('',#3037,#3035,#1913,.T.);
#3712=EDGE_CURVE('',#3038,#3038,#2582,.T.);
#3713=EDGE_CURVE('',#3038,#3037,#1914,.T.);
#3714=EDGE_CURVE('',#3039,#3039,#2583,.T.);
#3715=EDGE_CURVE('',#3039,#3038,#1915,.T.);
#3716=EDGE_CURVE('',#3030,#3036,#1916,.T.);
#3717=EDGE_CURVE('',#3040,#3041,#2584,.T.);
#3718=EDGE_CURVE('',#3042,#3043,#2585,.T.);
#3719=EDGE_CURVE('',#3044,#3045,#2586,.T.);
#3720=EDGE_CURVE('',#3046,#3047,#2587,.T.);
#3721=EDGE_CURVE('',#3048,#3049,#2588,.T.);
#3722=EDGE_CURVE('',#3050,#3051,#2589,.T.);
#3723=EDGE_CURVE('',#3052,#3053,#2590,.T.);
#3724=EDGE_CURVE('',#3054,#3055,#2591,.T.);
#3725=EDGE_CURVE('',#3056,#3057,#334,.T.);
#3726=EDGE_CURVE('',#3058,#3056,#2592,.T.);
#3727=EDGE_CURVE('',#3059,#3058,#335,.T.);
#3728=EDGE_CURVE('',#3057,#3059,#2593,.T.);
#3729=EDGE_CURVE('',#3060,#3058,#2594,.T.);
#3730=EDGE_CURVE('',#3060,#3061,#336,.T.);
#3731=EDGE_CURVE('',#3062,#3061,#2595,.T.);
#3732=EDGE_CURVE('',#3062,#3063,#337,.T.);
#3733=EDGE_CURVE('',#3064,#3063,#2596,.T.);
#3734=EDGE_CURVE('',#3064,#3065,#338,.T.);
#3735=EDGE_CURVE('',#3065,#3066,#1917,.T.);
#3736=EDGE_CURVE('',#3066,#3066,#2597,.T.);
#3737=EDGE_CURVE('',#3065,#3067,#339,.T.);
#3738=EDGE_CURVE('',#3068,#3067,#2598,.T.);
#3739=EDGE_CURVE('',#3068,#3069,#340,.T.);
#3740=EDGE_CURVE('',#3070,#3069,#2599,.T.);
#3741=EDGE_CURVE('',#3070,#3071,#341,.T.);
#3742=EDGE_CURVE('',#3072,#3071,#2600,.T.);
#3743=EDGE_CURVE('',#3072,#3073,#342,.T.);
#3744=EDGE_CURVE('',#3074,#3073,#2601,.T.);
#3745=EDGE_CURVE('',#3074,#3075,#343,.T.);
#3746=EDGE_CURVE('',#3059,#3075,#2602,.T.);
#3747=EDGE_CURVE('',#3056,#3076,#2603,.T.);
#3748=EDGE_CURVE('',#3076,#3060,#2604,.T.);
#3749=EDGE_CURVE('',#3077,#3076,#344,.T.);
#3750=EDGE_CURVE('',#3061,#3077,#2605,.T.);
#3751=EDGE_CURVE('',#3077,#3078,#2606,.T.);
#3752=EDGE_CURVE('',#3078,#3062,#2607,.T.);
#3753=EDGE_CURVE('',#3079,#3078,#345,.T.);
#3754=EDGE_CURVE('',#3063,#3079,#2608,.T.);
#3755=EDGE_CURVE('',#3079,#3080,#2609,.T.);
#3756=EDGE_CURVE('',#3080,#3064,#2610,.T.);
#3757=EDGE_CURVE('',#3081,#3082,#346,.T.);
#3758=EDGE_CURVE('',#3067,#3081,#2611,.T.);
#3759=EDGE_CURVE('',#3082,#3080,#347,.T.);
#3760=EDGE_CURVE('',#3081,#3083,#2612,.T.);
#3761=EDGE_CURVE('',#3083,#3068,#2613,.T.);
#3762=EDGE_CURVE('',#3084,#3083,#348,.T.);
#3763=EDGE_CURVE('',#3069,#3084,#2614,.T.);
#3764=EDGE_CURVE('',#3084,#3085,#2615,.T.);
#3765=EDGE_CURVE('',#3085,#3070,#2616,.T.);
#3766=EDGE_CURVE('',#3086,#3085,#349,.T.);
#3767=EDGE_CURVE('',#3071,#3086,#2617,.T.);
#3768=EDGE_CURVE('',#3086,#3087,#2618,.T.);
#3769=EDGE_CURVE('',#3087,#3072,#2619,.T.);
#3770=EDGE_CURVE('',#3088,#3087,#350,.T.);
#3771=EDGE_CURVE('',#3073,#3088,#2620,.T.);
#3772=EDGE_CURVE('',#3089,#3089,#2621,.T.);
#3773=EDGE_CURVE('',#3089,#3082,#1918,.T.);
#3774=EDGE_CURVE('',#3090,#3057,#2622,.T.);
#3775=EDGE_CURVE('',#3090,#3091,#351,.T.);
#3776=EDGE_CURVE('',#3088,#3091,#2623,.T.);
#3777=EDGE_CURVE('',#3075,#3090,#2624,.T.);
#3778=EDGE_CURVE('',#3091,#3074,#2625,.T.);
#3779=EDGE_CURVE('',#3092,#3092,#2626,.T.);
#3780=EDGE_CURVE('',#3093,#3093,#2627,.T.);
#3781=EDGE_CURVE('',#3094,#3094,#2628,.T.);
#3782=EDGE_CURVE('',#3094,#3092,#1919,.T.);
#3783=EDGE_CURVE('',#3095,#3095,#2629,.T.);
#3784=EDGE_CURVE('',#3095,#3093,#1920,.T.);
#3785=EDGE_CURVE('',#3096,#3096,#2630,.T.);
#3786=EDGE_CURVE('',#3097,#3097,#2631,.T.);
#3787=EDGE_CURVE('',#3098,#3098,#2632,.T.);
#3788=EDGE_CURVE('',#3098,#3096,#1921,.T.);
#3789=EDGE_CURVE('',#3099,#3099,#2633,.T.);
#3790=EDGE_CURVE('',#3099,#3097,#1922,.T.);
#3791=EDGE_CURVE('',#3100,#3100,#2634,.T.);
#3792=EDGE_CURVE('',#3101,#3101,#2635,.T.);
#3793=EDGE_CURVE('',#3102,#3102,#2636,.T.);
#3794=EDGE_CURVE('',#3102,#3101,#1923,.T.);
#3795=EDGE_CURVE('',#3103,#3103,#2637,.T.);
#3796=EDGE_CURVE('',#3103,#3102,#1924,.T.);
#3797=EDGE_CURVE('',#3104,#3104,#2638,.T.);
#3798=EDGE_CURVE('',#3104,#3103,#1925,.T.);
#3799=EDGE_CURVE('',#3105,#3105,#2639,.T.);
#3800=EDGE_CURVE('',#3106,#3106,#2640,.F.);
#3801=EDGE_CURVE('',#3106,#3105,#1926,.T.);
#3802=EDGE_CURVE('',#3100,#3106,#1927,.T.);
#3803=EDGE_CURVE('',#3107,#3108,#1928,.T.);
#3804=EDGE_CURVE('',#3108,#3109,#1929,.T.);
#3805=EDGE_CURVE('',#3109,#3110,#1930,.T.);
#3806=EDGE_CURVE('',#3107,#3110,#1931,.T.);
#3807=EDGE_CURVE('',#3108,#3111,#1932,.T.);
#3808=EDGE_CURVE('',#3111,#3112,#1933,.T.);
#3809=EDGE_CURVE('',#3112,#3109,#1934,.T.);
#3810=EDGE_CURVE('',#3111,#3113,#1935,.T.);
#3811=EDGE_CURVE('',#3113,#3114,#1936,.T.);
#3812=EDGE_CURVE('',#3114,#3112,#1937,.T.);
#3813=EDGE_CURVE('',#3113,#3115,#1938,.T.);
#3814=EDGE_CURVE('',#3115,#3116,#1939,.T.);
#3815=EDGE_CURVE('',#3116,#3114,#1940,.T.);
#3816=EDGE_CURVE('',#3115,#3117,#1941,.T.);
#3817=EDGE_CURVE('',#3117,#3118,#1942,.T.);
#3818=EDGE_CURVE('',#3118,#3116,#1943,.T.);
#3819=EDGE_CURVE('',#3117,#3107,#1944,.T.);
#3820=EDGE_CURVE('',#3110,#3118,#1945,.T.);
#3821=EDGE_CURVE('',#3119,#3119,#2641,.T.);
#3822=EDGE_CURVE('',#3119,#3120,#1946,.T.);
#3823=EDGE_CURVE('',#3120,#3120,#2642,.T.);
#3824=EDGE_CURVE('',#3121,#3121,#2643,.T.);
#3825=EDGE_CURVE('',#3121,#3122,#1947,.T.);
#3826=EDGE_CURVE('',#3122,#3122,#2644,.T.);
#3827=EDGE_CURVE('',#3123,#3123,#2645,.T.);
#3828=EDGE_CURVE('',#3124,#3124,#2646,.T.);
#3829=EDGE_CURVE('',#3125,#3125,#2647,.T.);
#3830=EDGE_CURVE('',#3125,#3123,#1948,.T.);
#3831=EDGE_CURVE('',#3124,#3126,#1949,.T.);
#3832=EDGE_CURVE('',#3126,#3126,#2648,.T.);
#3833=EDGE_CURVE('',#3127,#3128,#1950,.T.);
#3834=EDGE_CURVE('',#3127,#3128,#2649,.T.);
#3835=EDGE_CURVE('',#3129,#3127,#352,.T.);
#3836=EDGE_CURVE('',#3130,#3129,#2650,.T.);
#3837=EDGE_CURVE('',#3131,#3130,#353,.T.);
#3838=EDGE_CURVE('',#3131,#3132,#1951,.T.);
#3839=EDGE_CURVE('',#3133,#3132,#354,.T.);
#3840=EDGE_CURVE('',#3132,#3133,#355,.T.);
#3841=EDGE_CURVE('',#3128,#3131,#356,.T.);
#3842=EDGE_CURVE('',#3130,#3129,#1952,.T.);
#3843=EDGE_CURVE('',#3134,#3134,#2651,.T.);
#3844=EDGE_CURVE('',#3134,#3135,#1953,.T.);
#3845=EDGE_CURVE('',#3135,#3135,#2652,.T.);
#3846=EDGE_CURVE('',#3136,#3136,#2653,.T.);
#3847=EDGE_CURVE('',#3136,#3137,#1954,.T.);
#3848=EDGE_CURVE('',#3137,#3137,#2654,.T.);
#3849=EDGE_CURVE('',#3138,#3138,#2655,.T.);
#3850=EDGE_CURVE('',#3138,#3139,#1955,.T.);
#3851=EDGE_CURVE('',#3139,#3139,#2656,.T.);
#3852=EDGE_CURVE('',#3140,#3140,#2657,.T.);
#3853=EDGE_CURVE('',#3140,#3141,#1956,.T.);
#3854=EDGE_CURVE('',#3141,#3141,#2658,.T.);
#3855=EDGE_CURVE('',#3142,#3142,#2659,.T.);
#3856=EDGE_CURVE('',#3142,#3143,#1957,.T.);
#3857=EDGE_CURVE('',#3143,#3143,#2660,.T.);
#3858=EDGE_CURVE('',#3144,#3144,#2661,.T.);
#3859=EDGE_CURVE('',#3144,#3145,#1958,.T.);
#3860=EDGE_CURVE('',#3145,#3145,#2662,.T.);
#3861=EDGE_CURVE('',#3146,#3146,#2663,.T.);
#3862=EDGE_CURVE('',#3146,#3147,#1959,.T.);
#3863=EDGE_CURVE('',#3147,#3147,#2664,.T.);
#3864=EDGE_CURVE('',#3148,#3148,#2665,.T.);
#3865=EDGE_CURVE('',#3148,#3149,#1960,.T.);
#3866=EDGE_CURVE('',#3149,#3149,#2666,.T.);
#3867=EDGE_CURVE('',#3150,#3150,#2667,.T.);
#3868=EDGE_CURVE('',#3150,#3151,#1961,.T.);
#3869=EDGE_CURVE('',#3151,#3151,#2668,.T.);
#3870=EDGE_CURVE('',#3152,#3152,#2669,.T.);
#3871=EDGE_CURVE('',#3152,#3153,#1962,.T.);
#3872=EDGE_CURVE('',#3153,#3153,#2670,.T.);
#3873=EDGE_CURVE('',#3154,#3154,#2671,.T.);
#3874=EDGE_CURVE('',#3155,#3156,#1963,.T.);
#3875=EDGE_CURVE('',#3155,#3157,#1964,.T.);
#3876=EDGE_CURVE('',#3157,#3158,#1965,.T.);
#3877=EDGE_CURVE('',#3156,#3158,#1966,.T.);
#3878=EDGE_CURVE('',#3159,#3155,#1967,.T.);
#3879=EDGE_CURVE('',#3159,#3160,#1968,.T.);
#3880=EDGE_CURVE('',#3160,#3157,#1969,.T.);
#3881=EDGE_CURVE('',#3161,#3159,#1970,.T.);
#3882=EDGE_CURVE('',#3161,#3162,#1971,.T.);
#3883=EDGE_CURVE('',#3162,#3160,#1972,.T.);
#3884=EDGE_CURVE('',#3163,#3161,#1973,.T.);
#3885=EDGE_CURVE('',#3163,#3164,#1974,.T.);
#3886=EDGE_CURVE('',#3164,#3162,#1975,.T.);
#3887=EDGE_CURVE('',#3165,#3163,#1976,.T.);
#3888=EDGE_CURVE('',#3165,#3166,#1977,.T.);
#3889=EDGE_CURVE('',#3166,#3164,#1978,.T.);
#3890=EDGE_CURVE('',#3156,#3165,#1979,.T.);
#3891=EDGE_CURVE('',#3158,#3166,#1980,.T.);
#3892=EDGE_CURVE('',#3167,#3167,#2672,.T.);
#3893=EDGE_CURVE('',#3168,#3168,#2673,.T.);
#3894=EDGE_CURVE('',#3168,#3167,#1981,.T.);
#3895=EDGE_CURVE('',#3154,#3168,#1982,.T.);
#3896=EDGE_CURVE('',#3169,#3170,#357,.T.);
#3897=EDGE_CURVE('',#3171,#3169,#358,.T.);
#3898=EDGE_CURVE('',#3170,#3171,#359,.T.);
#3899=EDGE_CURVE('',#3170,#3172,#1983,.T.);
#3900=EDGE_CURVE('',#3173,#3172,#360,.T.);
#3901=EDGE_CURVE('',#3174,#3173,#361,.T.);
#3902=EDGE_CURVE('',#3175,#3174,#362,.T.);
#3903=EDGE_CURVE('',#3172,#3175,#363,.T.);
#3904=EDGE_CURVE('',#3176,#3177,#364,.T.);
#3905=EDGE_CURVE('',#3177,#3176,#365,.T.);
#3906=EDGE_CURVE('',#3177,#3178,#1984,.T.);
#3907=EDGE_CURVE('',#3179,#3178,#366,.T.);
#3908=EDGE_CURVE('',#3180,#3179,#367,.T.);
#3909=EDGE_CURVE('',#3178,#3180,#368,.T.);
#3910=EDGE_CURVE('',#3181,#3181,#2674,.T.);
#3911=EDGE_CURVE('',#3181,#3171,#1985,.T.);
#3912=EDGE_CURVE('',#3169,#3182,#1986,.T.);
#3913=EDGE_CURVE('',#3182,#3182,#2675,.T.);
#3914=EDGE_CURVE('',#3183,#3184,#369,.T.);
#3915=EDGE_CURVE('',#3184,#3185,#370,.T.);
#3916=EDGE_CURVE('',#3185,#3183,#371,.T.);
#3917=EDGE_CURVE('',#3186,#3187,#372,.T.);
#3918=EDGE_CURVE('',#3187,#3188,#373,.T.);
#3919=EDGE_CURVE('',#3188,#3186,#374,.T.);
#3920=EDGE_CURVE('',#3185,#3189,#1987,.T.);
#3921=EDGE_CURVE('',#3190,#3189,#375,.T.);
#3922=EDGE_CURVE('',#3189,#3190,#376,.T.);
#3923=EDGE_CURVE('',#3191,#3192,#377,.T.);
#3924=EDGE_CURVE('',#3192,#3191,#378,.T.);
#3925=EDGE_CURVE('',#3192,#3188,#1988,.T.);
#3926=EDGE_CURVE('',#3193,#3193,#2676,.T.);
#3927=EDGE_CURVE('',#3193,#3173,#1989,.T.);
#3928=EDGE_CURVE('',#3175,#3194,#1990,.T.);
#3929=EDGE_CURVE('',#3194,#3194,#2677,.T.);
#3930=EDGE_CURVE('',#3195,#3195,#2678,.T.);
#3931=EDGE_CURVE('',#3196,#3197,#2679,.T.);
#3932=EDGE_CURVE('',#3198,#3197,#2680,.T.);
#3933=EDGE_CURVE('',#3198,#3199,#2681,.T.);
#3934=EDGE_CURVE('',#3200,#3199,#2682,.T.);
#3935=EDGE_CURVE('',#3200,#3201,#2683,.T.);
#3936=EDGE_CURVE('',#3202,#3201,#2684,.T.);
#3937=EDGE_CURVE('',#3202,#3203,#2685,.T.);
#3938=EDGE_CURVE('',#3204,#3203,#2686,.T.);
#3939=EDGE_CURVE('',#3204,#3205,#2687,.T.);
#3940=EDGE_CURVE('',#3206,#3205,#2688,.T.);
#3941=EDGE_CURVE('',#3206,#3207,#2689,.T.);
#3942=EDGE_CURVE('',#3208,#3207,#2690,.T.);
#3943=EDGE_CURVE('',#3208,#3209,#2691,.T.);
#3944=EDGE_CURVE('',#3210,#3209,#2692,.T.);
#3945=EDGE_CURVE('',#3210,#3211,#2693,.T.);
#3946=EDGE_CURVE('',#3212,#3211,#2694,.T.);
#3947=EDGE_CURVE('',#3212,#3213,#2695,.T.);
#3948=EDGE_CURVE('',#3214,#3213,#2696,.T.);
#3949=EDGE_CURVE('',#3214,#3215,#2697,.T.);
#3950=EDGE_CURVE('',#3216,#3215,#2698,.T.);
#3951=EDGE_CURVE('',#3216,#3217,#2699,.T.);
#3952=EDGE_CURVE('',#3218,#3217,#2700,.T.);
#3953=EDGE_CURVE('',#3218,#3219,#2701,.T.);
#3954=EDGE_CURVE('',#3220,#3219,#2702,.T.);
#3955=EDGE_CURVE('',#3220,#3221,#2703,.T.);
#3956=EDGE_CURVE('',#3222,#3221,#2704,.T.);
#3957=EDGE_CURVE('',#3222,#3223,#2705,.T.);
#3958=EDGE_CURVE('',#3224,#3223,#2706,.T.);
#3959=EDGE_CURVE('',#3224,#3225,#2707,.T.);
#3960=EDGE_CURVE('',#3226,#3225,#2708,.T.);
#3961=EDGE_CURVE('',#3226,#3227,#2709,.T.);
#3962=EDGE_CURVE('',#3228,#3227,#2710,.T.);
#3963=EDGE_CURVE('',#3228,#3229,#2711,.T.);
#3964=EDGE_CURVE('',#3230,#3229,#2712,.T.);
#3965=EDGE_CURVE('',#3230,#3231,#2713,.T.);
#3966=EDGE_CURVE('',#3232,#3231,#2714,.T.);
#3967=EDGE_CURVE('',#3232,#3233,#2715,.T.);
#3968=EDGE_CURVE('',#3234,#3233,#2716,.T.);
#3969=EDGE_CURVE('',#3234,#3235,#2717,.T.);
#3970=EDGE_CURVE('',#3196,#3235,#2718,.T.);
#3971=EDGE_CURVE('',#3236,#3236,#2719,.T.);
#3972=EDGE_CURVE('',#3236,#3195,#1991,.T.);
#3973=EDGE_CURVE('',#3237,#3237,#2720,.T.);
#3974=EDGE_CURVE('',#3238,#3239,#2721,.T.);
#3975=EDGE_CURVE('',#3239,#3240,#2722,.T.);
#3976=EDGE_CURVE('',#3240,#3241,#2723,.T.);
#3977=EDGE_CURVE('',#3241,#3242,#2724,.T.);
#3978=EDGE_CURVE('',#3242,#3243,#2725,.T.);
#3979=EDGE_CURVE('',#3243,#3244,#2726,.T.);
#3980=EDGE_CURVE('',#3244,#3245,#2727,.T.);
#3981=EDGE_CURVE('',#3245,#3246,#2728,.T.);
#3982=EDGE_CURVE('',#3246,#3247,#2729,.T.);
#3983=EDGE_CURVE('',#3247,#3248,#2730,.T.);
#3984=EDGE_CURVE('',#3248,#3249,#2731,.T.);
#3985=EDGE_CURVE('',#3249,#3250,#2732,.T.);
#3986=EDGE_CURVE('',#3250,#3251,#2733,.T.);
#3987=EDGE_CURVE('',#3251,#3252,#2734,.T.);
#3988=EDGE_CURVE('',#3252,#3253,#2735,.T.);
#3989=EDGE_CURVE('',#3253,#3254,#2736,.T.);
#3990=EDGE_CURVE('',#3254,#3255,#2737,.T.);
#3991=EDGE_CURVE('',#3255,#3256,#2738,.T.);
#3992=EDGE_CURVE('',#3256,#3257,#2739,.T.);
#3993=EDGE_CURVE('',#3257,#3258,#2740,.T.);
#3994=EDGE_CURVE('',#3258,#3259,#2741,.T.);
#3995=EDGE_CURVE('',#3259,#3260,#2742,.T.);
#3996=EDGE_CURVE('',#3260,#3261,#2743,.T.);
#3997=EDGE_CURVE('',#3261,#3262,#2744,.T.);
#3998=EDGE_CURVE('',#3262,#3263,#2745,.T.);
#3999=EDGE_CURVE('',#3263,#3264,#2746,.T.);
#4000=EDGE_CURVE('',#3264,#3265,#2747,.T.);
#4001=EDGE_CURVE('',#3265,#3266,#2748,.T.);
#4002=EDGE_CURVE('',#3266,#3267,#2749,.T.);
#4003=EDGE_CURVE('',#3267,#3268,#2750,.T.);
#4004=EDGE_CURVE('',#3268,#3269,#2751,.T.);
#4005=EDGE_CURVE('',#3269,#3270,#2752,.T.);
#4006=EDGE_CURVE('',#3270,#3271,#2753,.T.);
#4007=EDGE_CURVE('',#3271,#3272,#2754,.T.);
#4008=EDGE_CURVE('',#3272,#3273,#2755,.T.);
#4009=EDGE_CURVE('',#3273,#3274,#2756,.T.);
#4010=EDGE_CURVE('',#3274,#3275,#2757,.T.);
#4011=EDGE_CURVE('',#3275,#3276,#2758,.T.);
#4012=EDGE_CURVE('',#3276,#3277,#2759,.T.);
#4013=EDGE_CURVE('',#3277,#3238,#2760,.T.);
#4014=EDGE_CURVE('',#3278,#3278,#2761,.T.);
#4015=EDGE_CURVE('',#3278,#3237,#1992,.T.);
#4016=EDGE_CURVE('',#3239,#3196,#1993,.T.);
#4017=EDGE_CURVE('',#3197,#3238,#1994,.T.);
#4018=EDGE_CURVE('',#3277,#3198,#1995,.T.);
#4019=EDGE_CURVE('',#3199,#3276,#1996,.T.);
#4020=EDGE_CURVE('',#3275,#3200,#1997,.T.);
#4021=EDGE_CURVE('',#3201,#3274,#1998,.T.);
#4022=EDGE_CURVE('',#3273,#3202,#1999,.T.);
#4023=EDGE_CURVE('',#3203,#3272,#2000,.T.);
#4024=EDGE_CURVE('',#3271,#3204,#2001,.T.);
#4025=EDGE_CURVE('',#3205,#3270,#2002,.T.);
#4026=EDGE_CURVE('',#3269,#3206,#2003,.T.);
#4027=EDGE_CURVE('',#3207,#3268,#2004,.T.);
#4028=EDGE_CURVE('',#3267,#3208,#2005,.T.);
#4029=EDGE_CURVE('',#3209,#3266,#2006,.T.);
#4030=EDGE_CURVE('',#3265,#3210,#2007,.T.);
#4031=EDGE_CURVE('',#3211,#3264,#2008,.T.);
#4032=EDGE_CURVE('',#3263,#3212,#2009,.T.);
#4033=EDGE_CURVE('',#3213,#3262,#2010,.T.);
#4034=EDGE_CURVE('',#3261,#3214,#2011,.T.);
#4035=EDGE_CURVE('',#3215,#3260,#2012,.T.);
#4036=EDGE_CURVE('',#3259,#3216,#2013,.T.);
#4037=EDGE_CURVE('',#3217,#3258,#2014,.T.);
#4038=EDGE_CURVE('',#3257,#3218,#2015,.T.);
#4039=EDGE_CURVE('',#3219,#3256,#2016,.T.);
#4040=EDGE_CURVE('',#3255,#3220,#2017,.T.);
#4041=EDGE_CURVE('',#3221,#3254,#2018,.T.);
#4042=EDGE_CURVE('',#3253,#3222,#2019,.T.);
#4043=EDGE_CURVE('',#3223,#3252,#2020,.T.);
#4044=EDGE_CURVE('',#3251,#3224,#2021,.T.);
#4045=EDGE_CURVE('',#3225,#3250,#2022,.T.);
#4046=EDGE_CURVE('',#3249,#3226,#2023,.T.);
#4047=EDGE_CURVE('',#3227,#3248,#2024,.T.);
#4048=EDGE_CURVE('',#3247,#3228,#2025,.T.);
#4049=EDGE_CURVE('',#3229,#3246,#2026,.T.);
#4050=EDGE_CURVE('',#3245,#3230,#2027,.T.);
#4051=EDGE_CURVE('',#3231,#3244,#2028,.T.);
#4052=EDGE_CURVE('',#3243,#3232,#2029,.T.);
#4053=EDGE_CURVE('',#3233,#3242,#2030,.T.);
#4054=EDGE_CURVE('',#3235,#3240,#2031,.T.);
#4055=EDGE_CURVE('',#3241,#3234,#2032,.T.);
#4056=EDGE_CURVE('',#3279,#3280,#2033,.T.);
#4057=EDGE_CURVE('',#3280,#3281,#2034,.T.);
#4058=EDGE_CURVE('',#3281,#3282,#2035,.T.);
#4059=EDGE_CURVE('',#3279,#3282,#2036,.T.);
#4060=EDGE_CURVE('',#3280,#3283,#2037,.T.);
#4061=EDGE_CURVE('',#3283,#3284,#2038,.T.);
#4062=EDGE_CURVE('',#3284,#3281,#2039,.T.);
#4063=EDGE_CURVE('',#3283,#3285,#2040,.T.);
#4064=EDGE_CURVE('',#3285,#3286,#2041,.T.);
#4065=EDGE_CURVE('',#3286,#3284,#2042,.T.);
#4066=EDGE_CURVE('',#3285,#3287,#2043,.T.);
#4067=EDGE_CURVE('',#3287,#3288,#2044,.T.);
#4068=EDGE_CURVE('',#3288,#3286,#2045,.T.);
#4069=EDGE_CURVE('',#3287,#3289,#2046,.T.);
#4070=EDGE_CURVE('',#3289,#3290,#2047,.T.);
#4071=EDGE_CURVE('',#3290,#3288,#2048,.T.);
#4072=EDGE_CURVE('',#3289,#3279,#2049,.T.);
#4073=EDGE_CURVE('',#3282,#3290,#2050,.T.);
#4074=EDGE_CURVE('',#3291,#3291,#2762,.T.);
#4075=EDGE_CURVE('',#3292,#3292,#2763,.T.);
#4076=EDGE_CURVE('',#3293,#3293,#2764,.T.);
#4077=EDGE_CURVE('',#3293,#3292,#2051,.T.);
#4078=EDGE_CURVE('',#3294,#3294,#2765,.T.);
#4079=EDGE_CURVE('',#3294,#3293,#2052,.T.);
#4080=EDGE_CURVE('',#3295,#3295,#2766,.T.);
#4081=EDGE_CURVE('',#3295,#3294,#2053,.T.);
#4082=EDGE_CURVE('',#3296,#3296,#2767,.T.);
#4083=EDGE_CURVE('',#3297,#3297,#2768,.F.);
#4084=EDGE_CURVE('',#3297,#3296,#2054,.T.);
#4085=EDGE_CURVE('',#3291,#3297,#2055,.T.);
#4086=ORIENTED_EDGE('',*,*,#3298,.F.);
#4087=ORIENTED_EDGE('',*,*,#3299,.T.);
#4088=ORIENTED_EDGE('',*,*,#3300,.F.);
#4089=ORIENTED_EDGE('',*,*,#3299,.F.);
#4090=ORIENTED_EDGE('',*,*,#3301,.F.);
#4091=ORIENTED_EDGE('',*,*,#3302,.T.);
#4092=ORIENTED_EDGE('',*,*,#3303,.F.);
#4093=ORIENTED_EDGE('',*,*,#3302,.F.);
#4094=ORIENTED_EDGE('',*,*,#3304,.F.);
#4095=ORIENTED_EDGE('',*,*,#3305,.T.);
#4096=ORIENTED_EDGE('',*,*,#3306,.F.);
#4097=ORIENTED_EDGE('',*,*,#3305,.F.);
#4098=ORIENTED_EDGE('',*,*,#3307,.F.);
#4099=ORIENTED_EDGE('',*,*,#3308,.T.);
#4100=ORIENTED_EDGE('',*,*,#3309,.F.);
#4101=ORIENTED_EDGE('',*,*,#3308,.F.);
#4102=ORIENTED_EDGE('',*,*,#3310,.F.);
#4103=ORIENTED_EDGE('',*,*,#3311,.T.);
#4104=ORIENTED_EDGE('',*,*,#3312,.F.);
#4105=ORIENTED_EDGE('',*,*,#3311,.F.);
#4106=ORIENTED_EDGE('',*,*,#3313,.T.);
#4107=ORIENTED_EDGE('',*,*,#3314,.T.);
#4108=ORIENTED_EDGE('',*,*,#3315,.F.);
#4109=ORIENTED_EDGE('',*,*,#3316,.F.);
#4110=ORIENTED_EDGE('',*,*,#3317,.T.);
#4111=ORIENTED_EDGE('',*,*,#3316,.T.);
#4112=ORIENTED_EDGE('',*,*,#3318,.F.);
#4113=ORIENTED_EDGE('',*,*,#3319,.F.);
#4114=ORIENTED_EDGE('',*,*,#3320,.T.);
#4115=ORIENTED_EDGE('',*,*,#3319,.T.);
#4116=ORIENTED_EDGE('',*,*,#3321,.F.);
#4117=ORIENTED_EDGE('',*,*,#3322,.F.);
#4118=ORIENTED_EDGE('',*,*,#3323,.T.);
#4119=ORIENTED_EDGE('',*,*,#3322,.T.);
#4120=ORIENTED_EDGE('',*,*,#3324,.F.);
#4121=ORIENTED_EDGE('',*,*,#3314,.F.);
#4122=ORIENTED_EDGE('',*,*,#3324,.T.);
#4123=ORIENTED_EDGE('',*,*,#3321,.T.);
#4124=ORIENTED_EDGE('',*,*,#3318,.T.);
#4125=ORIENTED_EDGE('',*,*,#3315,.T.);
#4126=ORIENTED_EDGE('',*,*,#3300,.T.);
#4127=ORIENTED_EDGE('',*,*,#3303,.T.);
#4128=ORIENTED_EDGE('',*,*,#3306,.T.);
#4129=ORIENTED_EDGE('',*,*,#3309,.T.);
#4130=ORIENTED_EDGE('',*,*,#3312,.T.);
#4131=ORIENTED_EDGE('',*,*,#3323,.F.);
#4132=ORIENTED_EDGE('',*,*,#3313,.F.);
#4133=ORIENTED_EDGE('',*,*,#3317,.F.);
#4134=ORIENTED_EDGE('',*,*,#3320,.F.);
#4135=ORIENTED_EDGE('',*,*,#3298,.T.);
#4136=ORIENTED_EDGE('',*,*,#3301,.T.);
#4137=ORIENTED_EDGE('',*,*,#3304,.T.);
#4138=ORIENTED_EDGE('',*,*,#3307,.T.);
#4139=ORIENTED_EDGE('',*,*,#3310,.T.);
#4140=ORIENTED_EDGE('',*,*,#3325,.T.);
#4141=ORIENTED_EDGE('',*,*,#3326,.T.);
#4142=ORIENTED_EDGE('',*,*,#3327,.F.);
#4143=ORIENTED_EDGE('',*,*,#3328,.F.);
#4144=ORIENTED_EDGE('',*,*,#3329,.T.);
#4145=ORIENTED_EDGE('',*,*,#3328,.T.);
#4146=ORIENTED_EDGE('',*,*,#3330,.F.);
#4147=ORIENTED_EDGE('',*,*,#3331,.F.);
#4148=ORIENTED_EDGE('',*,*,#3332,.T.);
#4149=ORIENTED_EDGE('',*,*,#3331,.T.);
#4150=ORIENTED_EDGE('',*,*,#3333,.F.);
#4151=ORIENTED_EDGE('',*,*,#3334,.F.);
#4152=ORIENTED_EDGE('',*,*,#3335,.T.);
#4153=ORIENTED_EDGE('',*,*,#3334,.T.);
#4154=ORIENTED_EDGE('',*,*,#3336,.F.);
#4155=ORIENTED_EDGE('',*,*,#3326,.F.);
#4156=ORIENTED_EDGE('',*,*,#3336,.T.);
#4157=ORIENTED_EDGE('',*,*,#3333,.T.);
#4158=ORIENTED_EDGE('',*,*,#3330,.T.);
#4159=ORIENTED_EDGE('',*,*,#3327,.T.);
#4160=ORIENTED_EDGE('',*,*,#3335,.F.);
#4161=ORIENTED_EDGE('',*,*,#3325,.F.);
#4162=ORIENTED_EDGE('',*,*,#3329,.F.);
#4163=ORIENTED_EDGE('',*,*,#3332,.F.);
#4164=ORIENTED_EDGE('',*,*,#3337,.T.);
#4165=ORIENTED_EDGE('',*,*,#3338,.T.);
#4166=ORIENTED_EDGE('',*,*,#3339,.F.);
#4167=ORIENTED_EDGE('',*,*,#3340,.F.);
#4168=ORIENTED_EDGE('',*,*,#3341,.T.);
#4169=ORIENTED_EDGE('',*,*,#3340,.T.);
#4170=ORIENTED_EDGE('',*,*,#3342,.F.);
#4171=ORIENTED_EDGE('',*,*,#3343,.F.);
#4172=ORIENTED_EDGE('',*,*,#3344,.T.);
#4173=ORIENTED_EDGE('',*,*,#3343,.T.);
#4174=ORIENTED_EDGE('',*,*,#3345,.F.);
#4175=ORIENTED_EDGE('',*,*,#3346,.F.);
#4176=ORIENTED_EDGE('',*,*,#3347,.T.);
#4177=ORIENTED_EDGE('',*,*,#3346,.T.);
#4178=ORIENTED_EDGE('',*,*,#3348,.F.);
#4179=ORIENTED_EDGE('',*,*,#3338,.F.);
#4180=ORIENTED_EDGE('',*,*,#3348,.T.);
#4181=ORIENTED_EDGE('',*,*,#3345,.T.);
#4182=ORIENTED_EDGE('',*,*,#3342,.T.);
#4183=ORIENTED_EDGE('',*,*,#3339,.T.);
#4184=ORIENTED_EDGE('',*,*,#3347,.F.);
#4185=ORIENTED_EDGE('',*,*,#3337,.F.);
#4186=ORIENTED_EDGE('',*,*,#3341,.F.);
#4187=ORIENTED_EDGE('',*,*,#3344,.F.);
#4188=ORIENTED_EDGE('',*,*,#3349,.F.);
#4189=ORIENTED_EDGE('',*,*,#3350,.T.);
#4190=ORIENTED_EDGE('',*,*,#3351,.F.);
#4191=ORIENTED_EDGE('',*,*,#3350,.F.);
#4192=ORIENTED_EDGE('',*,*,#3352,.F.);
#4193=ORIENTED_EDGE('',*,*,#3353,.T.);
#4194=ORIENTED_EDGE('',*,*,#3354,.F.);
#4195=ORIENTED_EDGE('',*,*,#3353,.F.);
#4196=ORIENTED_EDGE('',*,*,#3355,.F.);
#4197=ORIENTED_EDGE('',*,*,#3356,.T.);
#4198=ORIENTED_EDGE('',*,*,#3357,.F.);
#4199=ORIENTED_EDGE('',*,*,#3356,.F.);
#4200=ORIENTED_EDGE('',*,*,#3358,.T.);
#4201=ORIENTED_EDGE('',*,*,#3359,.F.);
#4202=ORIENTED_EDGE('',*,*,#3358,.F.);
#4203=ORIENTED_EDGE('',*,*,#3360,.T.);
#4204=ORIENTED_EDGE('',*,*,#3361,.F.);
#4205=ORIENTED_EDGE('',*,*,#3360,.F.);
#4206=ORIENTED_EDGE('',*,*,#3362,.F.);
#4207=ORIENTED_EDGE('',*,*,#3363,.T.);
#4208=ORIENTED_EDGE('',*,*,#3359,.T.);
#4209=ORIENTED_EDGE('',*,*,#3363,.F.);
#4210=ORIENTED_EDGE('',*,*,#3362,.T.);
#4211=ORIENTED_EDGE('',*,*,#3364,.T.);
#4212=ORIENTED_EDGE('',*,*,#3351,.T.);
#4213=ORIENTED_EDGE('',*,*,#3354,.T.);
#4214=ORIENTED_EDGE('',*,*,#3357,.T.);
#4215=ORIENTED_EDGE('',*,*,#3365,.F.);
#4216=ORIENTED_EDGE('',*,*,#3364,.F.);
#4217=ORIENTED_EDGE('',*,*,#3366,.T.);
#4218=ORIENTED_EDGE('',*,*,#3367,.T.);
#4219=ORIENTED_EDGE('',*,*,#3366,.F.);
#4220=ORIENTED_EDGE('',*,*,#3368,.F.);
#4221=ORIENTED_EDGE('',*,*,#3369,.T.);
#4222=ORIENTED_EDGE('',*,*,#3365,.T.);
#4223=ORIENTED_EDGE('',*,*,#3369,.F.);
#4224=ORIENTED_EDGE('',*,*,#3368,.T.);
#4225=ORIENTED_EDGE('',*,*,#3361,.T.);
#4226=ORIENTED_EDGE('',*,*,#3367,.F.);
#4227=ORIENTED_EDGE('',*,*,#3349,.T.);
#4228=ORIENTED_EDGE('',*,*,#3352,.T.);
#4229=ORIENTED_EDGE('',*,*,#3355,.T.);
#4230=ORIENTED_EDGE('',*,*,#3370,.F.);
#4231=ORIENTED_EDGE('',*,*,#3371,.T.);
#4232=ORIENTED_EDGE('',*,*,#3372,.F.);
#4233=ORIENTED_EDGE('',*,*,#3373,.F.);
#4234=ORIENTED_EDGE('',*,*,#3374,.F.);
#4235=ORIENTED_EDGE('',*,*,#3375,.T.);
#4236=ORIENTED_EDGE('',*,*,#3376,.F.);
#4237=ORIENTED_EDGE('',*,*,#3377,.F.);
#4238=ORIENTED_EDGE('',*,*,#3375,.F.);
#4239=ORIENTED_EDGE('',*,*,#3378,.F.);
#4240=ORIENTED_EDGE('',*,*,#3371,.F.);
#4241=ORIENTED_EDGE('',*,*,#3379,.F.);
#4242=ORIENTED_EDGE('',*,*,#3373,.T.);
#4243=ORIENTED_EDGE('',*,*,#3380,.F.);
#4244=ORIENTED_EDGE('',*,*,#3381,.T.);
#4245=ORIENTED_EDGE('',*,*,#3382,.T.);
#4246=ORIENTED_EDGE('',*,*,#3381,.F.);
#4247=ORIENTED_EDGE('',*,*,#3378,.T.);
#4248=ORIENTED_EDGE('',*,*,#3374,.T.);
#4249=ORIENTED_EDGE('',*,*,#3379,.T.);
#4250=ORIENTED_EDGE('',*,*,#3372,.T.);
#4251=ORIENTED_EDGE('',*,*,#3370,.T.);
#4252=ORIENTED_EDGE('',*,*,#3383,.F.);
#4253=ORIENTED_EDGE('',*,*,#3384,.T.);
#4254=ORIENTED_EDGE('',*,*,#3385,.T.);
#4255=ORIENTED_EDGE('',*,*,#3384,.F.);
#4256=ORIENTED_EDGE('',*,*,#3376,.T.);
#4257=ORIENTED_EDGE('',*,*,#3377,.T.);
#4258=ORIENTED_EDGE('',*,*,#3383,.T.);
#4259=ORIENTED_EDGE('',*,*,#3380,.T.);
#4260=ORIENTED_EDGE('',*,*,#3385,.F.);
#4261=ORIENTED_EDGE('',*,*,#3382,.F.);
#4262=ORIENTED_EDGE('',*,*,#3386,.F.);
#4263=ORIENTED_EDGE('',*,*,#3387,.T.);
#4264=ORIENTED_EDGE('',*,*,#3388,.T.);
#4265=ORIENTED_EDGE('',*,*,#3387,.F.);
#4266=ORIENTED_EDGE('',*,*,#3388,.F.);
#4267=ORIENTED_EDGE('',*,*,#3389,.F.);
#4268=ORIENTED_EDGE('',*,*,#3390,.T.);
#4269=ORIENTED_EDGE('',*,*,#3391,.F.);
#4270=ORIENTED_EDGE('',*,*,#3390,.F.);
#4271=ORIENTED_EDGE('',*,*,#3392,.F.);
#4272=ORIENTED_EDGE('',*,*,#3393,.T.);
#4273=ORIENTED_EDGE('',*,*,#3394,.T.);
#4274=ORIENTED_EDGE('',*,*,#3393,.F.);
#4275=ORIENTED_EDGE('',*,*,#3391,.T.);
#4276=ORIENTED_EDGE('',*,*,#3389,.T.);
#4277=ORIENTED_EDGE('',*,*,#3392,.T.);
#4278=ORIENTED_EDGE('',*,*,#3394,.F.);
#4279=ORIENTED_EDGE('',*,*,#3386,.T.);
#4280=ORIENTED_EDGE('',*,*,#3395,.F.);
#4281=ORIENTED_EDGE('',*,*,#3396,.T.);
#4282=ORIENTED_EDGE('',*,*,#3397,.F.);
#4283=ORIENTED_EDGE('',*,*,#3398,.T.);
#4284=ORIENTED_EDGE('',*,*,#3396,.F.);
#4285=ORIENTED_EDGE('',*,*,#3395,.T.);
#4286=ORIENTED_EDGE('',*,*,#3399,.F.);
#4287=ORIENTED_EDGE('',*,*,#3398,.F.);
#4288=ORIENTED_EDGE('',*,*,#3399,.T.);
#4289=ORIENTED_EDGE('',*,*,#3400,.T.);
#4290=ORIENTED_EDGE('',*,*,#3401,.T.);
#4291=ORIENTED_EDGE('',*,*,#3402,.T.);
#4292=ORIENTED_EDGE('',*,*,#3403,.F.);
#4293=ORIENTED_EDGE('',*,*,#3404,.F.);
#4294=ORIENTED_EDGE('',*,*,#3405,.F.);
#4295=ORIENTED_EDGE('',*,*,#3400,.F.);
#4296=ORIENTED_EDGE('',*,*,#3397,.T.);
#4297=ORIENTED_EDGE('',*,*,#3401,.F.);
#4298=ORIENTED_EDGE('',*,*,#3405,.T.);
#4299=ORIENTED_EDGE('',*,*,#3406,.F.);
#4300=ORIENTED_EDGE('',*,*,#3402,.F.);
#4301=ORIENTED_EDGE('',*,*,#3406,.T.);
#4302=ORIENTED_EDGE('',*,*,#3407,.T.);
#4303=ORIENTED_EDGE('',*,*,#3408,.T.);
#4304=ORIENTED_EDGE('',*,*,#3409,.T.);
#4305=ORIENTED_EDGE('',*,*,#3410,.T.);
#4306=ORIENTED_EDGE('',*,*,#3411,.T.);
#4307=ORIENTED_EDGE('',*,*,#3403,.T.);
#4308=ORIENTED_EDGE('',*,*,#3407,.F.);
#4309=ORIENTED_EDGE('',*,*,#3404,.T.);
#4310=ORIENTED_EDGE('',*,*,#3411,.F.);
#4311=ORIENTED_EDGE('',*,*,#3410,.F.);
#4312=ORIENTED_EDGE('',*,*,#3412,.T.);
#4313=ORIENTED_EDGE('',*,*,#3413,.F.);
#4314=ORIENTED_EDGE('',*,*,#3408,.F.);
#4315=ORIENTED_EDGE('',*,*,#3414,.T.);
#4316=ORIENTED_EDGE('',*,*,#3415,.T.);
#4317=ORIENTED_EDGE('',*,*,#3414,.F.);
#4318=ORIENTED_EDGE('',*,*,#3416,.F.);
#4319=ORIENTED_EDGE('',*,*,#3413,.T.);
#4320=ORIENTED_EDGE('',*,*,#3415,.F.);
#4321=ORIENTED_EDGE('',*,*,#3416,.T.);
#4322=ORIENTED_EDGE('',*,*,#3412,.F.);
#4323=ORIENTED_EDGE('',*,*,#3409,.F.);
#4324=ORIENTED_EDGE('',*,*,#3417,.F.);
#4325=ORIENTED_EDGE('',*,*,#3418,.T.);
#4326=ORIENTED_EDGE('',*,*,#3419,.T.);
#4327=ORIENTED_EDGE('',*,*,#3418,.F.);
#4328=ORIENTED_EDGE('',*,*,#3419,.F.);
#4329=ORIENTED_EDGE('',*,*,#3420,.F.);
#4330=ORIENTED_EDGE('',*,*,#3421,.T.);
#4331=ORIENTED_EDGE('',*,*,#3422,.F.);
#4332=ORIENTED_EDGE('',*,*,#3421,.F.);
#4333=ORIENTED_EDGE('',*,*,#3423,.T.);
#4334=ORIENTED_EDGE('',*,*,#3424,.T.);
#4335=ORIENTED_EDGE('',*,*,#3425,.F.);
#4336=ORIENTED_EDGE('',*,*,#3426,.F.);
#4337=ORIENTED_EDGE('',*,*,#3422,.T.);
#4338=ORIENTED_EDGE('',*,*,#3427,.T.);
#4339=ORIENTED_EDGE('',*,*,#3426,.T.);
#4340=ORIENTED_EDGE('',*,*,#3428,.F.);
#4341=ORIENTED_EDGE('',*,*,#3429,.F.);
#4342=ORIENTED_EDGE('',*,*,#3430,.T.);
#4343=ORIENTED_EDGE('',*,*,#3429,.T.);
#4344=ORIENTED_EDGE('',*,*,#3431,.F.);
#4345=ORIENTED_EDGE('',*,*,#3432,.F.);
#4346=ORIENTED_EDGE('',*,*,#3420,.T.);
#4347=ORIENTED_EDGE('',*,*,#3433,.T.);
#4348=ORIENTED_EDGE('',*,*,#3432,.T.);
#4349=ORIENTED_EDGE('',*,*,#3434,.F.);
#4350=ORIENTED_EDGE('',*,*,#3424,.F.);
#4351=ORIENTED_EDGE('',*,*,#3434,.T.);
#4352=ORIENTED_EDGE('',*,*,#3431,.T.);
#4353=ORIENTED_EDGE('',*,*,#3428,.T.);
#4354=ORIENTED_EDGE('',*,*,#3425,.T.);
#4355=ORIENTED_EDGE('',*,*,#3433,.F.);
#4356=ORIENTED_EDGE('',*,*,#3423,.F.);
#4357=ORIENTED_EDGE('',*,*,#3427,.F.);
#4358=ORIENTED_EDGE('',*,*,#3430,.F.);
#4359=ORIENTED_EDGE('',*,*,#3417,.T.);
#4360=ORIENTED_EDGE('',*,*,#3435,.T.);
#4361=ORIENTED_EDGE('',*,*,#3436,.T.);
#4362=ORIENTED_EDGE('',*,*,#3437,.T.);
#4363=ORIENTED_EDGE('',*,*,#3436,.F.);
#4364=ORIENTED_EDGE('',*,*,#3437,.F.);
#4365=ORIENTED_EDGE('',*,*,#3438,.T.);
#4366=ORIENTED_EDGE('',*,*,#3439,.T.);
#4367=ORIENTED_EDGE('',*,*,#3438,.F.);
#4368=ORIENTED_EDGE('',*,*,#3440,.T.);
#4369=ORIENTED_EDGE('',*,*,#3435,.F.);
#4370=ORIENTED_EDGE('',*,*,#3440,.F.);
#4371=ORIENTED_EDGE('',*,*,#3441,.T.);
#4372=ORIENTED_EDGE('',*,*,#3442,.T.);
#4373=ORIENTED_EDGE('',*,*,#3441,.F.);
#4374=ORIENTED_EDGE('',*,*,#3442,.F.);
#4375=ORIENTED_EDGE('',*,*,#3439,.F.);
#4376=ORIENTED_EDGE('',*,*,#3443,.F.);
#4377=ORIENTED_EDGE('',*,*,#3444,.F.);
#4378=ORIENTED_EDGE('',*,*,#3445,.T.);
#4379=ORIENTED_EDGE('',*,*,#3443,.T.);
#4380=ORIENTED_EDGE('',*,*,#3445,.F.);
#4381=ORIENTED_EDGE('',*,*,#3446,.F.);
#4382=ORIENTED_EDGE('',*,*,#3447,.T.);
#4383=ORIENTED_EDGE('',*,*,#3444,.T.);
#4384=ORIENTED_EDGE('',*,*,#3447,.F.);
#4385=ORIENTED_EDGE('',*,*,#3448,.F.);
#4386=ORIENTED_EDGE('',*,*,#3449,.T.);
#4387=ORIENTED_EDGE('',*,*,#3446,.T.);
#4388=ORIENTED_EDGE('',*,*,#3449,.F.);
#4389=ORIENTED_EDGE('',*,*,#3448,.T.);
#4390=ORIENTED_EDGE('',*,*,#3450,.F.);
#4391=ORIENTED_EDGE('',*,*,#3451,.F.);
#4392=ORIENTED_EDGE('',*,*,#3452,.T.);
#4393=ORIENTED_EDGE('',*,*,#3450,.T.);
#4394=ORIENTED_EDGE('',*,*,#3452,.F.);
#4395=ORIENTED_EDGE('',*,*,#3453,.F.);
#4396=ORIENTED_EDGE('',*,*,#3454,.T.);
#4397=ORIENTED_EDGE('',*,*,#3451,.T.);
#4398=ORIENTED_EDGE('',*,*,#3454,.F.);
#4399=ORIENTED_EDGE('',*,*,#3455,.F.);
#4400=ORIENTED_EDGE('',*,*,#3456,.T.);
#4401=ORIENTED_EDGE('',*,*,#3453,.T.);
#4402=ORIENTED_EDGE('',*,*,#3456,.F.);
#4403=ORIENTED_EDGE('',*,*,#3455,.T.);
#4404=ORIENTED_EDGE('',*,*,#3457,.T.);
#4405=ORIENTED_EDGE('',*,*,#3458,.T.);
#4406=ORIENTED_EDGE('',*,*,#3459,.T.);
#4407=ORIENTED_EDGE('',*,*,#3460,.F.);
#4408=ORIENTED_EDGE('',*,*,#3461,.T.);
#4409=ORIENTED_EDGE('',*,*,#3462,.T.);
#4410=ORIENTED_EDGE('',*,*,#3463,.T.);
#4411=ORIENTED_EDGE('',*,*,#3458,.F.);
#4412=ORIENTED_EDGE('',*,*,#3464,.T.);
#4413=ORIENTED_EDGE('',*,*,#3465,.T.);
#4414=ORIENTED_EDGE('',*,*,#3466,.T.);
#4415=ORIENTED_EDGE('',*,*,#3462,.F.);
#4416=ORIENTED_EDGE('',*,*,#3467,.T.);
#4417=ORIENTED_EDGE('',*,*,#3468,.T.);
#4418=ORIENTED_EDGE('',*,*,#3469,.T.);
#4419=ORIENTED_EDGE('',*,*,#3465,.F.);
#4420=ORIENTED_EDGE('',*,*,#3470,.T.);
#4421=ORIENTED_EDGE('',*,*,#3471,.T.);
#4422=ORIENTED_EDGE('',*,*,#3472,.T.);
#4423=ORIENTED_EDGE('',*,*,#3468,.F.);
#4424=ORIENTED_EDGE('',*,*,#3473,.T.);
#4425=ORIENTED_EDGE('',*,*,#3460,.T.);
#4426=ORIENTED_EDGE('',*,*,#3474,.T.);
#4427=ORIENTED_EDGE('',*,*,#3471,.F.);
#4428=ORIENTED_EDGE('',*,*,#3473,.F.);
#4429=ORIENTED_EDGE('',*,*,#3470,.F.);
#4430=ORIENTED_EDGE('',*,*,#3467,.F.);
#4431=ORIENTED_EDGE('',*,*,#3464,.F.);
#4432=ORIENTED_EDGE('',*,*,#3461,.F.);
#4433=ORIENTED_EDGE('',*,*,#3457,.F.);
#4434=ORIENTED_EDGE('',*,*,#3474,.F.);
#4435=ORIENTED_EDGE('',*,*,#3459,.F.);
#4436=ORIENTED_EDGE('',*,*,#3463,.F.);
#4437=ORIENTED_EDGE('',*,*,#3466,.F.);
#4438=ORIENTED_EDGE('',*,*,#3469,.F.);
#4439=ORIENTED_EDGE('',*,*,#3472,.F.);
#4440=ORIENTED_EDGE('',*,*,#3475,.F.);
#4441=ORIENTED_EDGE('',*,*,#3476,.F.);
#4442=ORIENTED_EDGE('',*,*,#3477,.T.);
#4443=ORIENTED_EDGE('',*,*,#3478,.F.);
#4444=ORIENTED_EDGE('',*,*,#3477,.F.);
#4445=ORIENTED_EDGE('',*,*,#3479,.F.);
#4446=ORIENTED_EDGE('',*,*,#3480,.F.);
#4447=ORIENTED_EDGE('',*,*,#3481,.F.);
#4448=ORIENTED_EDGE('',*,*,#3482,.F.);
#4449=ORIENTED_EDGE('',*,*,#3483,.F.);
#4450=ORIENTED_EDGE('',*,*,#3484,.T.);
#4451=ORIENTED_EDGE('',*,*,#3485,.F.);
#4452=ORIENTED_EDGE('',*,*,#3486,.F.);
#4453=ORIENTED_EDGE('',*,*,#3487,.F.);
#4454=ORIENTED_EDGE('',*,*,#3488,.F.);
#4455=ORIENTED_EDGE('',*,*,#3489,.F.);
#4456=ORIENTED_EDGE('',*,*,#3490,.F.);
#4457=ORIENTED_EDGE('',*,*,#3484,.F.);
#4458=ORIENTED_EDGE('',*,*,#3480,.T.);
#4459=ORIENTED_EDGE('',*,*,#3491,.T.);
#4460=ORIENTED_EDGE('',*,*,#3489,.T.);
#4461=ORIENTED_EDGE('',*,*,#3492,.F.);
#4462=ORIENTED_EDGE('',*,*,#3479,.T.);
#4463=ORIENTED_EDGE('',*,*,#3493,.T.);
#4464=ORIENTED_EDGE('',*,*,#3490,.T.);
#4465=ORIENTED_EDGE('',*,*,#3491,.F.);
#4466=ORIENTED_EDGE('',*,*,#3476,.T.);
#4467=ORIENTED_EDGE('',*,*,#3494,.T.);
#4468=ORIENTED_EDGE('',*,*,#3485,.T.);
#4469=ORIENTED_EDGE('',*,*,#3493,.F.);
#4470=ORIENTED_EDGE('',*,*,#3495,.F.);
#4471=ORIENTED_EDGE('',*,*,#3496,.T.);
#4472=ORIENTED_EDGE('',*,*,#3497,.T.);
#4473=ORIENTED_EDGE('',*,*,#3496,.F.);
#4474=ORIENTED_EDGE('',*,*,#3475,.T.);
#4475=ORIENTED_EDGE('',*,*,#3498,.T.);
#4476=ORIENTED_EDGE('',*,*,#3486,.T.);
#4477=ORIENTED_EDGE('',*,*,#3494,.F.);
#4478=ORIENTED_EDGE('',*,*,#3481,.T.);
#4479=ORIENTED_EDGE('',*,*,#3492,.T.);
#4480=ORIENTED_EDGE('',*,*,#3488,.T.);
#4481=ORIENTED_EDGE('',*,*,#3499,.F.);
#4482=ORIENTED_EDGE('',*,*,#3482,.T.);
#4483=ORIENTED_EDGE('',*,*,#3499,.T.);
#4484=ORIENTED_EDGE('',*,*,#3487,.T.);
#4485=ORIENTED_EDGE('',*,*,#3498,.F.);
#4486=ORIENTED_EDGE('',*,*,#3483,.T.);
#4487=ORIENTED_EDGE('',*,*,#3495,.T.);
#4488=ORIENTED_EDGE('',*,*,#3478,.T.);
#4489=ORIENTED_EDGE('',*,*,#3497,.F.);
#4490=ORIENTED_EDGE('',*,*,#3500,.F.);
#4491=ORIENTED_EDGE('',*,*,#3501,.F.);
#4492=ORIENTED_EDGE('',*,*,#3502,.T.);
#4493=ORIENTED_EDGE('',*,*,#3500,.T.);
#4494=ORIENTED_EDGE('',*,*,#3502,.F.);
#4495=ORIENTED_EDGE('',*,*,#3503,.F.);
#4496=ORIENTED_EDGE('',*,*,#3504,.T.);
#4497=ORIENTED_EDGE('',*,*,#3501,.T.);
#4498=ORIENTED_EDGE('',*,*,#3504,.F.);
#4499=ORIENTED_EDGE('',*,*,#3505,.F.);
#4500=ORIENTED_EDGE('',*,*,#3506,.T.);
#4501=ORIENTED_EDGE('',*,*,#3503,.T.);
#4502=ORIENTED_EDGE('',*,*,#3506,.F.);
#4503=ORIENTED_EDGE('',*,*,#3505,.T.);
#4504=ORIENTED_EDGE('',*,*,#3507,.F.);
#4505=ORIENTED_EDGE('',*,*,#3508,.F.);
#4506=ORIENTED_EDGE('',*,*,#3509,.T.);
#4507=ORIENTED_EDGE('',*,*,#3507,.T.);
#4508=ORIENTED_EDGE('',*,*,#3509,.F.);
#4509=ORIENTED_EDGE('',*,*,#3510,.F.);
#4510=ORIENTED_EDGE('',*,*,#3511,.T.);
#4511=ORIENTED_EDGE('',*,*,#3508,.T.);
#4512=ORIENTED_EDGE('',*,*,#3511,.F.);
#4513=ORIENTED_EDGE('',*,*,#3512,.F.);
#4514=ORIENTED_EDGE('',*,*,#3513,.T.);
#4515=ORIENTED_EDGE('',*,*,#3510,.T.);
#4516=ORIENTED_EDGE('',*,*,#3513,.F.);
#4517=ORIENTED_EDGE('',*,*,#3512,.T.);
#4518=ORIENTED_EDGE('',*,*,#3514,.T.);
#4519=ORIENTED_EDGE('',*,*,#3515,.T.);
#4520=ORIENTED_EDGE('',*,*,#3516,.T.);
#4521=ORIENTED_EDGE('',*,*,#3517,.F.);
#4522=ORIENTED_EDGE('',*,*,#3518,.T.);
#4523=ORIENTED_EDGE('',*,*,#3519,.T.);
#4524=ORIENTED_EDGE('',*,*,#3520,.T.);
#4525=ORIENTED_EDGE('',*,*,#3515,.F.);
#4526=ORIENTED_EDGE('',*,*,#3521,.T.);
#4527=ORIENTED_EDGE('',*,*,#3522,.T.);
#4528=ORIENTED_EDGE('',*,*,#3523,.T.);
#4529=ORIENTED_EDGE('',*,*,#3519,.F.);
#4530=ORIENTED_EDGE('',*,*,#3524,.T.);
#4531=ORIENTED_EDGE('',*,*,#3525,.T.);
#4532=ORIENTED_EDGE('',*,*,#3526,.T.);
#4533=ORIENTED_EDGE('',*,*,#3522,.F.);
#4534=ORIENTED_EDGE('',*,*,#3527,.T.);
#4535=ORIENTED_EDGE('',*,*,#3528,.T.);
#4536=ORIENTED_EDGE('',*,*,#3529,.T.);
#4537=ORIENTED_EDGE('',*,*,#3525,.F.);
#4538=ORIENTED_EDGE('',*,*,#3530,.T.);
#4539=ORIENTED_EDGE('',*,*,#3517,.T.);
#4540=ORIENTED_EDGE('',*,*,#3531,.T.);
#4541=ORIENTED_EDGE('',*,*,#3528,.F.);
#4542=ORIENTED_EDGE('',*,*,#3530,.F.);
#4543=ORIENTED_EDGE('',*,*,#3527,.F.);
#4544=ORIENTED_EDGE('',*,*,#3524,.F.);
#4545=ORIENTED_EDGE('',*,*,#3521,.F.);
#4546=ORIENTED_EDGE('',*,*,#3518,.F.);
#4547=ORIENTED_EDGE('',*,*,#3514,.F.);
#4548=ORIENTED_EDGE('',*,*,#3531,.F.);
#4549=ORIENTED_EDGE('',*,*,#3516,.F.);
#4550=ORIENTED_EDGE('',*,*,#3520,.F.);
#4551=ORIENTED_EDGE('',*,*,#3523,.F.);
#4552=ORIENTED_EDGE('',*,*,#3526,.F.);
#4553=ORIENTED_EDGE('',*,*,#3529,.F.);
#4554=ORIENTED_EDGE('',*,*,#3532,.F.);
#4555=ORIENTED_EDGE('',*,*,#3533,.T.);
#4556=ORIENTED_EDGE('',*,*,#3534,.F.);
#4557=ORIENTED_EDGE('',*,*,#3533,.F.);
#4558=ORIENTED_EDGE('',*,*,#3535,.F.);
#4559=ORIENTED_EDGE('',*,*,#3536,.T.);
#4560=ORIENTED_EDGE('',*,*,#3537,.F.);
#4561=ORIENTED_EDGE('',*,*,#3536,.F.);
#4562=ORIENTED_EDGE('',*,*,#3538,.F.);
#4563=ORIENTED_EDGE('',*,*,#3539,.T.);
#4564=ORIENTED_EDGE('',*,*,#3540,.F.);
#4565=ORIENTED_EDGE('',*,*,#3539,.F.);
#4566=ORIENTED_EDGE('',*,*,#3541,.F.);
#4567=ORIENTED_EDGE('',*,*,#3542,.T.);
#4568=ORIENTED_EDGE('',*,*,#3543,.F.);
#4569=ORIENTED_EDGE('',*,*,#3542,.F.);
#4570=ORIENTED_EDGE('',*,*,#3544,.F.);
#4571=ORIENTED_EDGE('',*,*,#3545,.T.);
#4572=ORIENTED_EDGE('',*,*,#3546,.F.);
#4573=ORIENTED_EDGE('',*,*,#3545,.F.);
#4574=ORIENTED_EDGE('',*,*,#3547,.F.);
#4575=ORIENTED_EDGE('',*,*,#3548,.T.);
#4576=ORIENTED_EDGE('',*,*,#3549,.F.);
#4577=ORIENTED_EDGE('',*,*,#3548,.F.);
#4578=ORIENTED_EDGE('',*,*,#3550,.F.);
#4579=ORIENTED_EDGE('',*,*,#3551,.T.);
#4580=ORIENTED_EDGE('',*,*,#3552,.F.);
#4581=ORIENTED_EDGE('',*,*,#3551,.F.);
#4582=ORIENTED_EDGE('',*,*,#3553,.F.);
#4583=ORIENTED_EDGE('',*,*,#3554,.T.);
#4584=ORIENTED_EDGE('',*,*,#3555,.F.);
#4585=ORIENTED_EDGE('',*,*,#3554,.F.);
#4586=ORIENTED_EDGE('',*,*,#3556,.F.);
#4587=ORIENTED_EDGE('',*,*,#3557,.T.);
#4588=ORIENTED_EDGE('',*,*,#3558,.F.);
#4589=ORIENTED_EDGE('',*,*,#3557,.F.);
#4590=ORIENTED_EDGE('',*,*,#3559,.F.);
#4591=ORIENTED_EDGE('',*,*,#3560,.T.);
#4592=ORIENTED_EDGE('',*,*,#3561,.F.);
#4593=ORIENTED_EDGE('',*,*,#3560,.F.);
#4594=ORIENTED_EDGE('',*,*,#3562,.F.);
#4595=ORIENTED_EDGE('',*,*,#3563,.F.);
#4596=ORIENTED_EDGE('',*,*,#3564,.F.);
#4597=ORIENTED_EDGE('',*,*,#3565,.T.);
#4598=ORIENTED_EDGE('',*,*,#3562,.T.);
#4599=ORIENTED_EDGE('',*,*,#3566,.T.);
#4600=ORIENTED_EDGE('',*,*,#3567,.F.);
#4601=ORIENTED_EDGE('',*,*,#3568,.F.);
#4602=ORIENTED_EDGE('',*,*,#3565,.F.);
#4603=ORIENTED_EDGE('',*,*,#3569,.F.);
#4604=ORIENTED_EDGE('',*,*,#3570,.F.);
#4605=ORIENTED_EDGE('',*,*,#3566,.F.);
#4606=ORIENTED_EDGE('',*,*,#3544,.T.);
#4607=ORIENTED_EDGE('',*,*,#3547,.T.);
#4608=ORIENTED_EDGE('',*,*,#3550,.T.);
#4609=ORIENTED_EDGE('',*,*,#3553,.T.);
#4610=ORIENTED_EDGE('',*,*,#3556,.T.);
#4611=ORIENTED_EDGE('',*,*,#3559,.T.);
#4612=ORIENTED_EDGE('',*,*,#3541,.T.);
#4613=ORIENTED_EDGE('',*,*,#3538,.T.);
#4614=ORIENTED_EDGE('',*,*,#3535,.T.);
#4615=ORIENTED_EDGE('',*,*,#3532,.T.);
#4616=ORIENTED_EDGE('',*,*,#3564,.T.);
#4617=ORIENTED_EDGE('',*,*,#3571,.F.);
#4618=ORIENTED_EDGE('',*,*,#3572,.F.);
#4619=ORIENTED_EDGE('',*,*,#3569,.T.);
#4620=ORIENTED_EDGE('',*,*,#3567,.T.);
#4621=ORIENTED_EDGE('',*,*,#3570,.T.);
#4622=ORIENTED_EDGE('',*,*,#3572,.T.);
#4623=ORIENTED_EDGE('',*,*,#3573,.F.);
#4624=ORIENTED_EDGE('',*,*,#3568,.T.);
#4625=ORIENTED_EDGE('',*,*,#3573,.T.);
#4626=ORIENTED_EDGE('',*,*,#3571,.T.);
#4627=ORIENTED_EDGE('',*,*,#3563,.T.);
#4628=ORIENTED_EDGE('',*,*,#3546,.T.);
#4629=ORIENTED_EDGE('',*,*,#3549,.T.);
#4630=ORIENTED_EDGE('',*,*,#3552,.T.);
#4631=ORIENTED_EDGE('',*,*,#3555,.T.);
#4632=ORIENTED_EDGE('',*,*,#3558,.T.);
#4633=ORIENTED_EDGE('',*,*,#3561,.T.);
#4634=ORIENTED_EDGE('',*,*,#3543,.T.);
#4635=ORIENTED_EDGE('',*,*,#3540,.T.);
#4636=ORIENTED_EDGE('',*,*,#3537,.T.);
#4637=ORIENTED_EDGE('',*,*,#3534,.T.);
#4638=ORIENTED_EDGE('',*,*,#3574,.F.);
#4639=ORIENTED_EDGE('',*,*,#3575,.T.);
#4640=ORIENTED_EDGE('',*,*,#3576,.F.);
#4641=ORIENTED_EDGE('',*,*,#3575,.F.);
#4642=ORIENTED_EDGE('',*,*,#3577,.F.);
#4643=ORIENTED_EDGE('',*,*,#3578,.T.);
#4644=ORIENTED_EDGE('',*,*,#3579,.F.);
#4645=ORIENTED_EDGE('',*,*,#3578,.F.);
#4646=ORIENTED_EDGE('',*,*,#3580,.F.);
#4647=ORIENTED_EDGE('',*,*,#3581,.T.);
#4648=ORIENTED_EDGE('',*,*,#3582,.F.);
#4649=ORIENTED_EDGE('',*,*,#3581,.F.);
#4650=ORIENTED_EDGE('',*,*,#3583,.F.);
#4651=ORIENTED_EDGE('',*,*,#3584,.T.);
#4652=ORIENTED_EDGE('',*,*,#3585,.F.);
#4653=ORIENTED_EDGE('',*,*,#3584,.F.);
#4654=ORIENTED_EDGE('',*,*,#3586,.F.);
#4655=ORIENTED_EDGE('',*,*,#3587,.T.);
#4656=ORIENTED_EDGE('',*,*,#3588,.F.);
#4657=ORIENTED_EDGE('',*,*,#3587,.F.);
#4658=ORIENTED_EDGE('',*,*,#3586,.T.);
#4659=ORIENTED_EDGE('',*,*,#3589,.T.);
#4660=ORIENTED_EDGE('',*,*,#3589,.F.);
#4661=ORIENTED_EDGE('',*,*,#3590,.T.);
#4662=ORIENTED_EDGE('',*,*,#3591,.T.);
#4663=ORIENTED_EDGE('',*,*,#3590,.F.);
#4664=ORIENTED_EDGE('',*,*,#3592,.F.);
#4665=ORIENTED_EDGE('',*,*,#3593,.T.);
#4666=ORIENTED_EDGE('',*,*,#3594,.T.);
#4667=ORIENTED_EDGE('',*,*,#3593,.F.);
#4668=ORIENTED_EDGE('',*,*,#3592,.T.);
#4669=ORIENTED_EDGE('',*,*,#3588,.T.);
#4670=ORIENTED_EDGE('',*,*,#3585,.T.);
#4671=ORIENTED_EDGE('',*,*,#3582,.T.);
#4672=ORIENTED_EDGE('',*,*,#3579,.T.);
#4673=ORIENTED_EDGE('',*,*,#3576,.T.);
#4674=ORIENTED_EDGE('',*,*,#3594,.F.);
#4675=ORIENTED_EDGE('',*,*,#3591,.F.);
#4676=ORIENTED_EDGE('',*,*,#3583,.T.);
#4677=ORIENTED_EDGE('',*,*,#3580,.T.);
#4678=ORIENTED_EDGE('',*,*,#3577,.T.);
#4679=ORIENTED_EDGE('',*,*,#3574,.T.);
#4680=ORIENTED_EDGE('',*,*,#3595,.F.);
#4681=ORIENTED_EDGE('',*,*,#3596,.T.);
#4682=ORIENTED_EDGE('',*,*,#3597,.F.);
#4683=ORIENTED_EDGE('',*,*,#3596,.F.);
#4684=ORIENTED_EDGE('',*,*,#3598,.F.);
#4685=ORIENTED_EDGE('',*,*,#3599,.T.);
#4686=ORIENTED_EDGE('',*,*,#3600,.F.);
#4687=ORIENTED_EDGE('',*,*,#3599,.F.);
#4688=ORIENTED_EDGE('',*,*,#3601,.F.);
#4689=ORIENTED_EDGE('',*,*,#3602,.T.);
#4690=ORIENTED_EDGE('',*,*,#3603,.F.);
#4691=ORIENTED_EDGE('',*,*,#3602,.F.);
#4692=ORIENTED_EDGE('',*,*,#3604,.F.);
#4693=ORIENTED_EDGE('',*,*,#3605,.T.);
#4694=ORIENTED_EDGE('',*,*,#3606,.F.);
#4695=ORIENTED_EDGE('',*,*,#3605,.F.);
#4696=ORIENTED_EDGE('',*,*,#3607,.F.);
#4697=ORIENTED_EDGE('',*,*,#3608,.T.);
#4698=ORIENTED_EDGE('',*,*,#3609,.T.);
#4699=ORIENTED_EDGE('',*,*,#3608,.F.);
#4700=ORIENTED_EDGE('',*,*,#3609,.F.);
#4701=ORIENTED_EDGE('',*,*,#3610,.F.);
#4702=ORIENTED_EDGE('',*,*,#3611,.F.);
#4703=ORIENTED_EDGE('',*,*,#3612,.T.);
#4704=ORIENTED_EDGE('',*,*,#3610,.T.);
#4705=ORIENTED_EDGE('',*,*,#3612,.F.);
#4706=ORIENTED_EDGE('',*,*,#3613,.F.);
#4707=ORIENTED_EDGE('',*,*,#3614,.T.);
#4708=ORIENTED_EDGE('',*,*,#3615,.T.);
#4709=ORIENTED_EDGE('',*,*,#3614,.F.);
#4710=ORIENTED_EDGE('',*,*,#3613,.T.);
#4711=ORIENTED_EDGE('',*,*,#3611,.T.);
#4712=ORIENTED_EDGE('',*,*,#3606,.T.);
#4713=ORIENTED_EDGE('',*,*,#3603,.T.);
#4714=ORIENTED_EDGE('',*,*,#3600,.T.);
#4715=ORIENTED_EDGE('',*,*,#3597,.T.);
#4716=ORIENTED_EDGE('',*,*,#3615,.F.);
#4717=ORIENTED_EDGE('',*,*,#3607,.T.);
#4718=ORIENTED_EDGE('',*,*,#3604,.T.);
#4719=ORIENTED_EDGE('',*,*,#3601,.T.);
#4720=ORIENTED_EDGE('',*,*,#3598,.T.);
#4721=ORIENTED_EDGE('',*,*,#3595,.T.);
#4722=ORIENTED_EDGE('',*,*,#3616,.F.);
#4723=ORIENTED_EDGE('',*,*,#3617,.T.);
#4724=ORIENTED_EDGE('',*,*,#3618,.F.);
#4725=ORIENTED_EDGE('',*,*,#3617,.F.);
#4726=ORIENTED_EDGE('',*,*,#3619,.F.);
#4727=ORIENTED_EDGE('',*,*,#3620,.T.);
#4728=ORIENTED_EDGE('',*,*,#3621,.F.);
#4729=ORIENTED_EDGE('',*,*,#3620,.F.);
#4730=ORIENTED_EDGE('',*,*,#3622,.F.);
#4731=ORIENTED_EDGE('',*,*,#3623,.T.);
#4732=ORIENTED_EDGE('',*,*,#3624,.F.);
#4733=ORIENTED_EDGE('',*,*,#3623,.F.);
#4734=ORIENTED_EDGE('',*,*,#3625,.F.);
#4735=ORIENTED_EDGE('',*,*,#3626,.T.);
#4736=ORIENTED_EDGE('',*,*,#3627,.F.);
#4737=ORIENTED_EDGE('',*,*,#3626,.F.);
#4738=ORIENTED_EDGE('',*,*,#3628,.F.);
#4739=ORIENTED_EDGE('',*,*,#3629,.T.);
#4740=ORIENTED_EDGE('',*,*,#3630,.F.);
#4741=ORIENTED_EDGE('',*,*,#3629,.F.);
#4742=ORIENTED_EDGE('',*,*,#3628,.T.);
#4743=ORIENTED_EDGE('',*,*,#3631,.T.);
#4744=ORIENTED_EDGE('',*,*,#3631,.F.);
#4745=ORIENTED_EDGE('',*,*,#3632,.T.);
#4746=ORIENTED_EDGE('',*,*,#3633,.T.);
#4747=ORIENTED_EDGE('',*,*,#3632,.F.);
#4748=ORIENTED_EDGE('',*,*,#3634,.F.);
#4749=ORIENTED_EDGE('',*,*,#3635,.T.);
#4750=ORIENTED_EDGE('',*,*,#3636,.T.);
#4751=ORIENTED_EDGE('',*,*,#3635,.F.);
#4752=ORIENTED_EDGE('',*,*,#3634,.T.);
#4753=ORIENTED_EDGE('',*,*,#3630,.T.);
#4754=ORIENTED_EDGE('',*,*,#3627,.T.);
#4755=ORIENTED_EDGE('',*,*,#3624,.T.);
#4756=ORIENTED_EDGE('',*,*,#3621,.T.);
#4757=ORIENTED_EDGE('',*,*,#3618,.T.);
#4758=ORIENTED_EDGE('',*,*,#3636,.F.);
#4759=ORIENTED_EDGE('',*,*,#3633,.F.);
#4760=ORIENTED_EDGE('',*,*,#3625,.T.);
#4761=ORIENTED_EDGE('',*,*,#3622,.T.);
#4762=ORIENTED_EDGE('',*,*,#3619,.T.);
#4763=ORIENTED_EDGE('',*,*,#3616,.T.);
#4764=ORIENTED_EDGE('',*,*,#3637,.F.);
#4765=ORIENTED_EDGE('',*,*,#3638,.T.);
#4766=ORIENTED_EDGE('',*,*,#3639,.F.);
#4767=ORIENTED_EDGE('',*,*,#3638,.F.);
#4768=ORIENTED_EDGE('',*,*,#3640,.F.);
#4769=ORIENTED_EDGE('',*,*,#3641,.T.);
#4770=ORIENTED_EDGE('',*,*,#3642,.F.);
#4771=ORIENTED_EDGE('',*,*,#3641,.F.);
#4772=ORIENTED_EDGE('',*,*,#3643,.F.);
#4773=ORIENTED_EDGE('',*,*,#3644,.T.);
#4774=ORIENTED_EDGE('',*,*,#3645,.F.);
#4775=ORIENTED_EDGE('',*,*,#3644,.F.);
#4776=ORIENTED_EDGE('',*,*,#3646,.F.);
#4777=ORIENTED_EDGE('',*,*,#3647,.T.);
#4778=ORIENTED_EDGE('',*,*,#3648,.F.);
#4779=ORIENTED_EDGE('',*,*,#3647,.F.);
#4780=ORIENTED_EDGE('',*,*,#3649,.F.);
#4781=ORIENTED_EDGE('',*,*,#3650,.T.);
#4782=ORIENTED_EDGE('',*,*,#3651,.T.);
#4783=ORIENTED_EDGE('',*,*,#3650,.F.);
#4784=ORIENTED_EDGE('',*,*,#3651,.F.);
#4785=ORIENTED_EDGE('',*,*,#3652,.F.);
#4786=ORIENTED_EDGE('',*,*,#3653,.F.);
#4787=ORIENTED_EDGE('',*,*,#3654,.T.);
#4788=ORIENTED_EDGE('',*,*,#3652,.T.);
#4789=ORIENTED_EDGE('',*,*,#3654,.F.);
#4790=ORIENTED_EDGE('',*,*,#3655,.F.);
#4791=ORIENTED_EDGE('',*,*,#3656,.T.);
#4792=ORIENTED_EDGE('',*,*,#3657,.T.);
#4793=ORIENTED_EDGE('',*,*,#3656,.F.);
#4794=ORIENTED_EDGE('',*,*,#3655,.T.);
#4795=ORIENTED_EDGE('',*,*,#3653,.T.);
#4796=ORIENTED_EDGE('',*,*,#3648,.T.);
#4797=ORIENTED_EDGE('',*,*,#3645,.T.);
#4798=ORIENTED_EDGE('',*,*,#3642,.T.);
#4799=ORIENTED_EDGE('',*,*,#3639,.T.);
#4800=ORIENTED_EDGE('',*,*,#3657,.F.);
#4801=ORIENTED_EDGE('',*,*,#3649,.T.);
#4802=ORIENTED_EDGE('',*,*,#3646,.T.);
#4803=ORIENTED_EDGE('',*,*,#3643,.T.);
#4804=ORIENTED_EDGE('',*,*,#3640,.T.);
#4805=ORIENTED_EDGE('',*,*,#3637,.T.);
#4806=ORIENTED_EDGE('',*,*,#3658,.F.);
#4807=ORIENTED_EDGE('',*,*,#3659,.F.);
#4808=ORIENTED_EDGE('',*,*,#3660,.F.);
#4809=ORIENTED_EDGE('',*,*,#3661,.T.);
#4810=ORIENTED_EDGE('',*,*,#3662,.F.);
#4811=ORIENTED_EDGE('',*,*,#3663,.F.);
#4812=ORIENTED_EDGE('',*,*,#3661,.F.);
#4813=ORIENTED_EDGE('',*,*,#3664,.F.);
#4814=ORIENTED_EDGE('',*,*,#3665,.T.);
#4815=ORIENTED_EDGE('',*,*,#3660,.T.);
#4816=ORIENTED_EDGE('',*,*,#3666,.T.);
#4817=ORIENTED_EDGE('',*,*,#3667,.F.);
#4818=ORIENTED_EDGE('',*,*,#3668,.F.);
#4819=ORIENTED_EDGE('',*,*,#3669,.F.);
#4820=ORIENTED_EDGE('',*,*,#3666,.F.);
#4821=ORIENTED_EDGE('',*,*,#3659,.T.);
#4822=ORIENTED_EDGE('',*,*,#3658,.T.);
#4823=ORIENTED_EDGE('',*,*,#3665,.F.);
#4824=ORIENTED_EDGE('',*,*,#3662,.T.);
#4825=ORIENTED_EDGE('',*,*,#3663,.T.);
#4826=ORIENTED_EDGE('',*,*,#3664,.T.);
#4827=ORIENTED_EDGE('',*,*,#3669,.T.);
#4828=ORIENTED_EDGE('',*,*,#3670,.T.);
#4829=ORIENTED_EDGE('',*,*,#3671,.T.);
#4830=ORIENTED_EDGE('',*,*,#3668,.T.);
#4831=ORIENTED_EDGE('',*,*,#3672,.T.);
#4832=ORIENTED_EDGE('',*,*,#3673,.T.);
#4833=ORIENTED_EDGE('',*,*,#3667,.T.);
#4834=ORIENTED_EDGE('',*,*,#3674,.T.);
#4835=ORIENTED_EDGE('',*,*,#3675,.T.);
#4836=ORIENTED_EDGE('',*,*,#3676,.T.);
#4837=ORIENTED_EDGE('',*,*,#3677,.T.);
#4838=ORIENTED_EDGE('',*,*,#3678,.T.);
#4839=ORIENTED_EDGE('',*,*,#3670,.F.);
#4840=ORIENTED_EDGE('',*,*,#3673,.F.);
#4841=ORIENTED_EDGE('',*,*,#3679,.F.);
#4842=ORIENTED_EDGE('',*,*,#3680,.T.);
#4843=ORIENTED_EDGE('',*,*,#3679,.T.);
#4844=ORIENTED_EDGE('',*,*,#3672,.F.);
#4845=ORIENTED_EDGE('',*,*,#3676,.F.);
#4846=ORIENTED_EDGE('',*,*,#3681,.F.);
#4847=ORIENTED_EDGE('',*,*,#3682,.T.);
#4848=ORIENTED_EDGE('',*,*,#3681,.T.);
#4849=ORIENTED_EDGE('',*,*,#3675,.F.);
#4850=ORIENTED_EDGE('',*,*,#3683,.F.);
#4851=ORIENTED_EDGE('',*,*,#3684,.T.);
#4852=ORIENTED_EDGE('',*,*,#3683,.T.);
#4853=ORIENTED_EDGE('',*,*,#3674,.F.);
#4854=ORIENTED_EDGE('',*,*,#3671,.F.);
#4855=ORIENTED_EDGE('',*,*,#3678,.F.);
#4856=ORIENTED_EDGE('',*,*,#3684,.F.);
#4857=ORIENTED_EDGE('',*,*,#3677,.F.);
#4858=ORIENTED_EDGE('',*,*,#3680,.F.);
#4859=ORIENTED_EDGE('',*,*,#3682,.F.);
#4860=ORIENTED_EDGE('',*,*,#3685,.F.);
#4861=ORIENTED_EDGE('',*,*,#3686,.F.);
#4862=ORIENTED_EDGE('',*,*,#3687,.T.);
#4863=ORIENTED_EDGE('',*,*,#3688,.F.);
#4864=ORIENTED_EDGE('',*,*,#3689,.F.);
#4865=ORIENTED_EDGE('',*,*,#3687,.F.);
#4866=ORIENTED_EDGE('',*,*,#3688,.T.);
#4867=ORIENTED_EDGE('',*,*,#3689,.T.);
#4868=ORIENTED_EDGE('',*,*,#3690,.T.);
#4869=ORIENTED_EDGE('',*,*,#3691,.T.);
#4870=ORIENTED_EDGE('',*,*,#3690,.F.);
#4871=ORIENTED_EDGE('',*,*,#3692,.T.);
#4872=ORIENTED_EDGE('',*,*,#3693,.T.);
#4873=ORIENTED_EDGE('',*,*,#3694,.F.);
#4874=ORIENTED_EDGE('',*,*,#3693,.F.);
#4875=ORIENTED_EDGE('',*,*,#3694,.T.);
#4876=ORIENTED_EDGE('',*,*,#3695,.T.);
#4877=ORIENTED_EDGE('',*,*,#3696,.F.);
#4878=ORIENTED_EDGE('',*,*,#3695,.F.);
#4879=ORIENTED_EDGE('',*,*,#3691,.F.);
#4880=ORIENTED_EDGE('',*,*,#3696,.T.);
#4881=ORIENTED_EDGE('',*,*,#3697,.F.);
#4882=ORIENTED_EDGE('',*,*,#3698,.T.);
#4883=ORIENTED_EDGE('',*,*,#3685,.T.);
#4884=ORIENTED_EDGE('',*,*,#3686,.T.);
#4885=ORIENTED_EDGE('',*,*,#3698,.F.);
#4886=ORIENTED_EDGE('',*,*,#3697,.T.);
#4887=ORIENTED_EDGE('',*,*,#3699,.F.);
#4888=ORIENTED_EDGE('',*,*,#3699,.T.);
#4889=ORIENTED_EDGE('',*,*,#3700,.T.);
#4890=ORIENTED_EDGE('',*,*,#3692,.F.);
#4891=ORIENTED_EDGE('',*,*,#3700,.F.);
#4892=ORIENTED_EDGE('',*,*,#3701,.F.);
#4893=ORIENTED_EDGE('',*,*,#3702,.F.);
#4894=ORIENTED_EDGE('',*,*,#3703,.T.);
#4895=ORIENTED_EDGE('',*,*,#3704,.F.);
#4896=ORIENTED_EDGE('',*,*,#3705,.F.);
#4897=ORIENTED_EDGE('',*,*,#3703,.F.);
#4898=ORIENTED_EDGE('',*,*,#3706,.T.);
#4899=ORIENTED_EDGE('',*,*,#3707,.T.);
#4900=ORIENTED_EDGE('',*,*,#3704,.T.);
#4901=ORIENTED_EDGE('',*,*,#3705,.T.);
#4902=ORIENTED_EDGE('',*,*,#3707,.F.);
#4903=ORIENTED_EDGE('',*,*,#3708,.F.);
#4904=ORIENTED_EDGE('',*,*,#3709,.T.);
#4905=ORIENTED_EDGE('',*,*,#3710,.F.);
#4906=ORIENTED_EDGE('',*,*,#3711,.T.);
#4907=ORIENTED_EDGE('',*,*,#3708,.T.);
#4908=ORIENTED_EDGE('',*,*,#3711,.F.);
#4909=ORIENTED_EDGE('',*,*,#3712,.F.);
#4910=ORIENTED_EDGE('',*,*,#3713,.T.);
#4911=ORIENTED_EDGE('',*,*,#3710,.T.);
#4912=ORIENTED_EDGE('',*,*,#3713,.F.);
#4913=ORIENTED_EDGE('',*,*,#3714,.F.);
#4914=ORIENTED_EDGE('',*,*,#3715,.T.);
#4915=ORIENTED_EDGE('',*,*,#3712,.T.);
#4916=ORIENTED_EDGE('',*,*,#3715,.F.);
#4917=ORIENTED_EDGE('',*,*,#3714,.T.);
#4918=ORIENTED_EDGE('',*,*,#3706,.F.);
#4919=ORIENTED_EDGE('',*,*,#3701,.T.);
#4920=ORIENTED_EDGE('',*,*,#3702,.T.);
#4921=ORIENTED_EDGE('',*,*,#3716,.T.);
#4922=ORIENTED_EDGE('',*,*,#3709,.F.);
#4923=ORIENTED_EDGE('',*,*,#3716,.F.);
#4924=ORIENTED_EDGE('',*,*,#3717,.T.);
#4925=ORIENTED_EDGE('',*,*,#3717,.F.);
#4926=ORIENTED_EDGE('',*,*,#3718,.T.);
#4927=ORIENTED_EDGE('',*,*,#3718,.F.);
#4928=ORIENTED_EDGE('',*,*,#3719,.T.);
#4929=ORIENTED_EDGE('',*,*,#3719,.F.);
#4930=ORIENTED_EDGE('',*,*,#3720,.T.);
#4931=ORIENTED_EDGE('',*,*,#3720,.F.);
#4932=ORIENTED_EDGE('',*,*,#3721,.T.);
#4933=ORIENTED_EDGE('',*,*,#3721,.F.);
#4934=ORIENTED_EDGE('',*,*,#3722,.T.);
#4935=ORIENTED_EDGE('',*,*,#3722,.F.);
#4936=ORIENTED_EDGE('',*,*,#3723,.T.);
#4937=ORIENTED_EDGE('',*,*,#3723,.F.);
#4938=ORIENTED_EDGE('',*,*,#3724,.T.);
#4939=ORIENTED_EDGE('',*,*,#3724,.F.);
#4940=ORIENTED_EDGE('',*,*,#3725,.F.);
#4941=ORIENTED_EDGE('',*,*,#3726,.F.);
#4942=ORIENTED_EDGE('',*,*,#3727,.F.);
#4943=ORIENTED_EDGE('',*,*,#3728,.F.);
#4944=ORIENTED_EDGE('',*,*,#3727,.T.);
#4945=ORIENTED_EDGE('',*,*,#3729,.F.);
#4946=ORIENTED_EDGE('',*,*,#3730,.T.);
#4947=ORIENTED_EDGE('',*,*,#3731,.F.);
#4948=ORIENTED_EDGE('',*,*,#3732,.T.);
#4949=ORIENTED_EDGE('',*,*,#3733,.F.);
#4950=ORIENTED_EDGE('',*,*,#3734,.T.);
#4951=ORIENTED_EDGE('',*,*,#3735,.T.);
#4952=ORIENTED_EDGE('',*,*,#3736,.F.);
#4953=ORIENTED_EDGE('',*,*,#3735,.F.);
#4954=ORIENTED_EDGE('',*,*,#3737,.T.);
#4955=ORIENTED_EDGE('',*,*,#3738,.F.);
#4956=ORIENTED_EDGE('',*,*,#3739,.T.);
#4957=ORIENTED_EDGE('',*,*,#3740,.F.);
#4958=ORIENTED_EDGE('',*,*,#3741,.T.);
#4959=ORIENTED_EDGE('',*,*,#3742,.F.);
#4960=ORIENTED_EDGE('',*,*,#3743,.T.);
#4961=ORIENTED_EDGE('',*,*,#3744,.F.);
#4962=ORIENTED_EDGE('',*,*,#3745,.T.);
#4963=ORIENTED_EDGE('',*,*,#3746,.F.);
#4964=ORIENTED_EDGE('',*,*,#3726,.T.);
#4965=ORIENTED_EDGE('',*,*,#3747,.T.);
#4966=ORIENTED_EDGE('',*,*,#3748,.T.);
#4967=ORIENTED_EDGE('',*,*,#3729,.T.);
#4968=ORIENTED_EDGE('',*,*,#3749,.F.);
#4969=ORIENTED_EDGE('',*,*,#3750,.F.);
#4970=ORIENTED_EDGE('',*,*,#3730,.F.);
#4971=ORIENTED_EDGE('',*,*,#3748,.F.);
#4972=ORIENTED_EDGE('',*,*,#3750,.T.);
#4973=ORIENTED_EDGE('',*,*,#3751,.T.);
#4974=ORIENTED_EDGE('',*,*,#3752,.T.);
#4975=ORIENTED_EDGE('',*,*,#3731,.T.);
#4976=ORIENTED_EDGE('',*,*,#3753,.F.);
#4977=ORIENTED_EDGE('',*,*,#3754,.F.);
#4978=ORIENTED_EDGE('',*,*,#3732,.F.);
#4979=ORIENTED_EDGE('',*,*,#3752,.F.);
#4980=ORIENTED_EDGE('',*,*,#3754,.T.);
#4981=ORIENTED_EDGE('',*,*,#3755,.T.);
#4982=ORIENTED_EDGE('',*,*,#3756,.T.);
#4983=ORIENTED_EDGE('',*,*,#3733,.T.);
#4984=ORIENTED_EDGE('',*,*,#3757,.F.);
#4985=ORIENTED_EDGE('',*,*,#3758,.F.);
#4986=ORIENTED_EDGE('',*,*,#3737,.F.);
#4987=ORIENTED_EDGE('',*,*,#3734,.F.);
#4988=ORIENTED_EDGE('',*,*,#3756,.F.);
#4989=ORIENTED_EDGE('',*,*,#3759,.F.);
#4990=ORIENTED_EDGE('',*,*,#3758,.T.);
#4991=ORIENTED_EDGE('',*,*,#3760,.T.);
#4992=ORIENTED_EDGE('',*,*,#3761,.T.);
#4993=ORIENTED_EDGE('',*,*,#3738,.T.);
#4994=ORIENTED_EDGE('',*,*,#3762,.F.);
#4995=ORIENTED_EDGE('',*,*,#3763,.F.);
#4996=ORIENTED_EDGE('',*,*,#3739,.F.);
#4997=ORIENTED_EDGE('',*,*,#3761,.F.);
#4998=ORIENTED_EDGE('',*,*,#3763,.T.);
#4999=ORIENTED_EDGE('',*,*,#3764,.T.);
#5000=ORIENTED_EDGE('',*,*,#3765,.T.);
#5001=ORIENTED_EDGE('',*,*,#3740,.T.);
#5002=ORIENTED_EDGE('',*,*,#3766,.F.);
#5003=ORIENTED_EDGE('',*,*,#3767,.F.);
#5004=ORIENTED_EDGE('',*,*,#3741,.F.);
#5005=ORIENTED_EDGE('',*,*,#3765,.F.);
#5006=ORIENTED_EDGE('',*,*,#3767,.T.);
#5007=ORIENTED_EDGE('',*,*,#3768,.T.);
#5008=ORIENTED_EDGE('',*,*,#3769,.T.);
#5009=ORIENTED_EDGE('',*,*,#3742,.T.);
#5010=ORIENTED_EDGE('',*,*,#3743,.F.);
#5011=ORIENTED_EDGE('',*,*,#3769,.F.);
#5012=ORIENTED_EDGE('',*,*,#3770,.F.);
#5013=ORIENTED_EDGE('',*,*,#3771,.F.);
#5014=ORIENTED_EDGE('',*,*,#3772,.F.);
#5015=ORIENTED_EDGE('',*,*,#3773,.T.);
#5016=ORIENTED_EDGE('',*,*,#3759,.T.);
#5017=ORIENTED_EDGE('',*,*,#3755,.F.);
#5018=ORIENTED_EDGE('',*,*,#3753,.T.);
#5019=ORIENTED_EDGE('',*,*,#3751,.F.);
#5020=ORIENTED_EDGE('',*,*,#3749,.T.);
#5021=ORIENTED_EDGE('',*,*,#3747,.F.);
#5022=ORIENTED_EDGE('',*,*,#3725,.T.);
#5023=ORIENTED_EDGE('',*,*,#3774,.F.);
#5024=ORIENTED_EDGE('',*,*,#3775,.T.);
#5025=ORIENTED_EDGE('',*,*,#3776,.F.);
#5026=ORIENTED_EDGE('',*,*,#3770,.T.);
#5027=ORIENTED_EDGE('',*,*,#3768,.F.);
#5028=ORIENTED_EDGE('',*,*,#3766,.T.);
#5029=ORIENTED_EDGE('',*,*,#3764,.F.);
#5030=ORIENTED_EDGE('',*,*,#3762,.T.);
#5031=ORIENTED_EDGE('',*,*,#3760,.F.);
#5032=ORIENTED_EDGE('',*,*,#3757,.T.);
#5033=ORIENTED_EDGE('',*,*,#3773,.F.);
#5034=ORIENTED_EDGE('',*,*,#3728,.T.);
#5035=ORIENTED_EDGE('',*,*,#3746,.T.);
#5036=ORIENTED_EDGE('',*,*,#3777,.T.);
#5037=ORIENTED_EDGE('',*,*,#3774,.T.);
#5038=ORIENTED_EDGE('',*,*,#3745,.F.);
#5039=ORIENTED_EDGE('',*,*,#3778,.F.);
#5040=ORIENTED_EDGE('',*,*,#3775,.F.);
#5041=ORIENTED_EDGE('',*,*,#3777,.F.);
#5042=ORIENTED_EDGE('',*,*,#3736,.T.);
#5043=ORIENTED_EDGE('',*,*,#3772,.T.);
#5044=ORIENTED_EDGE('',*,*,#3771,.T.);
#5045=ORIENTED_EDGE('',*,*,#3776,.T.);
#5046=ORIENTED_EDGE('',*,*,#3778,.T.);
#5047=ORIENTED_EDGE('',*,*,#3744,.T.);
#5048=ORIENTED_EDGE('',*,*,#3779,.F.);
#5049=ORIENTED_EDGE('',*,*,#3780,.T.);
#5050=ORIENTED_EDGE('',*,*,#3781,.F.);
#5051=ORIENTED_EDGE('',*,*,#3782,.T.);
#5052=ORIENTED_EDGE('',*,*,#3779,.T.);
#5053=ORIENTED_EDGE('',*,*,#3782,.F.);
#5054=ORIENTED_EDGE('',*,*,#3781,.T.);
#5055=ORIENTED_EDGE('',*,*,#3783,.F.);
#5056=ORIENTED_EDGE('',*,*,#3783,.T.);
#5057=ORIENTED_EDGE('',*,*,#3784,.T.);
#5058=ORIENTED_EDGE('',*,*,#3780,.F.);
#5059=ORIENTED_EDGE('',*,*,#3784,.F.);
#5060=ORIENTED_EDGE('',*,*,#3785,.F.);
#5061=ORIENTED_EDGE('',*,*,#3786,.T.);
#5062=ORIENTED_EDGE('',*,*,#3787,.F.);
#5063=ORIENTED_EDGE('',*,*,#3788,.T.);
#5064=ORIENTED_EDGE('',*,*,#3785,.T.);
#5065=ORIENTED_EDGE('',*,*,#3788,.F.);
#5066=ORIENTED_EDGE('',*,*,#3787,.T.);
#5067=ORIENTED_EDGE('',*,*,#3789,.F.);
#5068=ORIENTED_EDGE('',*,*,#3789,.T.);
#5069=ORIENTED_EDGE('',*,*,#3790,.T.);
#5070=ORIENTED_EDGE('',*,*,#3786,.F.);
#5071=ORIENTED_EDGE('',*,*,#3790,.F.);
#5072=ORIENTED_EDGE('',*,*,#3791,.F.);
#5073=ORIENTED_EDGE('',*,*,#3792,.F.);
#5074=ORIENTED_EDGE('',*,*,#3793,.F.);
#5075=ORIENTED_EDGE('',*,*,#3794,.T.);
#5076=ORIENTED_EDGE('',*,*,#3792,.T.);
#5077=ORIENTED_EDGE('',*,*,#3794,.F.);
#5078=ORIENTED_EDGE('',*,*,#3795,.F.);
#5079=ORIENTED_EDGE('',*,*,#3796,.T.);
#5080=ORIENTED_EDGE('',*,*,#3793,.T.);
#5081=ORIENTED_EDGE('',*,*,#3796,.F.);
#5082=ORIENTED_EDGE('',*,*,#3797,.F.);
#5083=ORIENTED_EDGE('',*,*,#3798,.T.);
#5084=ORIENTED_EDGE('',*,*,#3795,.T.);
#5085=ORIENTED_EDGE('',*,*,#3798,.F.);
#5086=ORIENTED_EDGE('',*,*,#3797,.T.);
#5087=ORIENTED_EDGE('',*,*,#3799,.F.);
#5088=ORIENTED_EDGE('',*,*,#3800,.F.);
#5089=ORIENTED_EDGE('',*,*,#3801,.T.);
#5090=ORIENTED_EDGE('',*,*,#3799,.T.);
#5091=ORIENTED_EDGE('',*,*,#3801,.F.);
#5092=ORIENTED_EDGE('',*,*,#3791,.T.);
#5093=ORIENTED_EDGE('',*,*,#3802,.T.);
#5094=ORIENTED_EDGE('',*,*,#3800,.T.);
#5095=ORIENTED_EDGE('',*,*,#3802,.F.);
#5096=ORIENTED_EDGE('',*,*,#3803,.T.);
#5097=ORIENTED_EDGE('',*,*,#3804,.T.);
#5098=ORIENTED_EDGE('',*,*,#3805,.T.);
#5099=ORIENTED_EDGE('',*,*,#3806,.F.);
#5100=ORIENTED_EDGE('',*,*,#3807,.T.);
#5101=ORIENTED_EDGE('',*,*,#3808,.T.);
#5102=ORIENTED_EDGE('',*,*,#3809,.T.);
#5103=ORIENTED_EDGE('',*,*,#3804,.F.);
#5104=ORIENTED_EDGE('',*,*,#3810,.T.);
#5105=ORIENTED_EDGE('',*,*,#3811,.T.);
#5106=ORIENTED_EDGE('',*,*,#3812,.T.);
#5107=ORIENTED_EDGE('',*,*,#3808,.F.);
#5108=ORIENTED_EDGE('',*,*,#3813,.T.);
#5109=ORIENTED_EDGE('',*,*,#3814,.T.);
#5110=ORIENTED_EDGE('',*,*,#3815,.T.);
#5111=ORIENTED_EDGE('',*,*,#3811,.F.);
#5112=ORIENTED_EDGE('',*,*,#3816,.T.);
#5113=ORIENTED_EDGE('',*,*,#3817,.T.);
#5114=ORIENTED_EDGE('',*,*,#3818,.T.);
#5115=ORIENTED_EDGE('',*,*,#3814,.F.);
#5116=ORIENTED_EDGE('',*,*,#3819,.T.);
#5117=ORIENTED_EDGE('',*,*,#3806,.T.);
#5118=ORIENTED_EDGE('',*,*,#3820,.T.);
#5119=ORIENTED_EDGE('',*,*,#3817,.F.);
#5120=ORIENTED_EDGE('',*,*,#3819,.F.);
#5121=ORIENTED_EDGE('',*,*,#3816,.F.);
#5122=ORIENTED_EDGE('',*,*,#3813,.F.);
#5123=ORIENTED_EDGE('',*,*,#3810,.F.);
#5124=ORIENTED_EDGE('',*,*,#3807,.F.);
#5125=ORIENTED_EDGE('',*,*,#3803,.F.);
#5126=ORIENTED_EDGE('',*,*,#3820,.F.);
#5127=ORIENTED_EDGE('',*,*,#3805,.F.);
#5128=ORIENTED_EDGE('',*,*,#3809,.F.);
#5129=ORIENTED_EDGE('',*,*,#3812,.F.);
#5130=ORIENTED_EDGE('',*,*,#3815,.F.);
#5131=ORIENTED_EDGE('',*,*,#3818,.F.);
#5132=ORIENTED_EDGE('',*,*,#3821,.F.);
#5133=ORIENTED_EDGE('',*,*,#3822,.T.);
#5134=ORIENTED_EDGE('',*,*,#3823,.F.);
#5135=ORIENTED_EDGE('',*,*,#3822,.F.);
#5136=ORIENTED_EDGE('',*,*,#3821,.T.);
#5137=ORIENTED_EDGE('',*,*,#3824,.F.);
#5138=ORIENTED_EDGE('',*,*,#3825,.T.);
#5139=ORIENTED_EDGE('',*,*,#3826,.F.);
#5140=ORIENTED_EDGE('',*,*,#3825,.F.);
#5141=ORIENTED_EDGE('',*,*,#3824,.T.);
#5142=ORIENTED_EDGE('',*,*,#3823,.T.);
#5143=ORIENTED_EDGE('',*,*,#3827,.F.);
#5144=ORIENTED_EDGE('',*,*,#3828,.F.);
#5145=ORIENTED_EDGE('',*,*,#3829,.F.);
#5146=ORIENTED_EDGE('',*,*,#3830,.T.);
#5147=ORIENTED_EDGE('',*,*,#3827,.T.);
#5148=ORIENTED_EDGE('',*,*,#3830,.F.);
#5149=ORIENTED_EDGE('',*,*,#3828,.T.);
#5150=ORIENTED_EDGE('',*,*,#3831,.T.);
#5151=ORIENTED_EDGE('',*,*,#3832,.T.);
#5152=ORIENTED_EDGE('',*,*,#3831,.F.);
#5153=ORIENTED_EDGE('',*,*,#3829,.T.);
#5154=ORIENTED_EDGE('',*,*,#3826,.T.);
#5155=ORIENTED_EDGE('',*,*,#3832,.F.);
#5156=ORIENTED_EDGE('',*,*,#3833,.F.);
#5157=ORIENTED_EDGE('',*,*,#3834,.T.);
#5158=ORIENTED_EDGE('',*,*,#3835,.F.);
#5159=ORIENTED_EDGE('',*,*,#3836,.F.);
#5160=ORIENTED_EDGE('',*,*,#3837,.F.);
#5161=ORIENTED_EDGE('',*,*,#3838,.T.);
#5162=ORIENTED_EDGE('',*,*,#3839,.F.);
#5163=ORIENTED_EDGE('',*,*,#3840,.F.);
#5164=ORIENTED_EDGE('',*,*,#3838,.F.);
#5165=ORIENTED_EDGE('',*,*,#3841,.F.);
#5166=ORIENTED_EDGE('',*,*,#3834,.F.);
#5167=ORIENTED_EDGE('',*,*,#3842,.F.);
#5168=ORIENTED_EDGE('',*,*,#3836,.T.);
#5169=ORIENTED_EDGE('',*,*,#3843,.F.);
#5170=ORIENTED_EDGE('',*,*,#3844,.T.);
#5171=ORIENTED_EDGE('',*,*,#3845,.T.);
#5172=ORIENTED_EDGE('',*,*,#3844,.F.);
#5173=ORIENTED_EDGE('',*,*,#3841,.T.);
#5174=ORIENTED_EDGE('',*,*,#3837,.T.);
#5175=ORIENTED_EDGE('',*,*,#3842,.T.);
#5176=ORIENTED_EDGE('',*,*,#3835,.T.);
#5177=ORIENTED_EDGE('',*,*,#3833,.T.);
#5178=ORIENTED_EDGE('',*,*,#3846,.F.);
#5179=ORIENTED_EDGE('',*,*,#3847,.T.);
#5180=ORIENTED_EDGE('',*,*,#3848,.T.);
#5181=ORIENTED_EDGE('',*,*,#3847,.F.);
#5182=ORIENTED_EDGE('',*,*,#3839,.T.);
#5183=ORIENTED_EDGE('',*,*,#3840,.T.);
#5184=ORIENTED_EDGE('',*,*,#3846,.T.);
#5185=ORIENTED_EDGE('',*,*,#3843,.T.);
#5186=ORIENTED_EDGE('',*,*,#3848,.F.);
#5187=ORIENTED_EDGE('',*,*,#3845,.F.);
#5188=ORIENTED_EDGE('',*,*,#3849,.F.);
#5189=ORIENTED_EDGE('',*,*,#3850,.T.);
#5190=ORIENTED_EDGE('',*,*,#3851,.T.);
#5191=ORIENTED_EDGE('',*,*,#3850,.F.);
#5192=ORIENTED_EDGE('',*,*,#3852,.F.);
#5193=ORIENTED_EDGE('',*,*,#3853,.T.);
#5194=ORIENTED_EDGE('',*,*,#3854,.T.);
#5195=ORIENTED_EDGE('',*,*,#3853,.F.);
#5196=ORIENTED_EDGE('',*,*,#3852,.T.);
#5197=ORIENTED_EDGE('',*,*,#3849,.T.);
#5198=ORIENTED_EDGE('',*,*,#3854,.F.);
#5199=ORIENTED_EDGE('',*,*,#3851,.F.);
#5200=ORIENTED_EDGE('',*,*,#3855,.F.);
#5201=ORIENTED_EDGE('',*,*,#3856,.T.);
#5202=ORIENTED_EDGE('',*,*,#3857,.T.);
#5203=ORIENTED_EDGE('',*,*,#3856,.F.);
#5204=ORIENTED_EDGE('',*,*,#3858,.F.);
#5205=ORIENTED_EDGE('',*,*,#3859,.T.);
#5206=ORIENTED_EDGE('',*,*,#3860,.T.);
#5207=ORIENTED_EDGE('',*,*,#3859,.F.);
#5208=ORIENTED_EDGE('',*,*,#3858,.T.);
#5209=ORIENTED_EDGE('',*,*,#3855,.T.);
#5210=ORIENTED_EDGE('',*,*,#3860,.F.);
#5211=ORIENTED_EDGE('',*,*,#3857,.F.);
#5212=ORIENTED_EDGE('',*,*,#3861,.F.);
#5213=ORIENTED_EDGE('',*,*,#3862,.T.);
#5214=ORIENTED_EDGE('',*,*,#3863,.T.);
#5215=ORIENTED_EDGE('',*,*,#3862,.F.);
#5216=ORIENTED_EDGE('',*,*,#3861,.T.);
#5217=ORIENTED_EDGE('',*,*,#3863,.F.);
#5218=ORIENTED_EDGE('',*,*,#3864,.F.);
#5219=ORIENTED_EDGE('',*,*,#3865,.T.);
#5220=ORIENTED_EDGE('',*,*,#3866,.T.);
#5221=ORIENTED_EDGE('',*,*,#3865,.F.);
#5222=ORIENTED_EDGE('',*,*,#3864,.T.);
#5223=ORIENTED_EDGE('',*,*,#3866,.F.);
#5224=ORIENTED_EDGE('',*,*,#3867,.F.);
#5225=ORIENTED_EDGE('',*,*,#3868,.T.);
#5226=ORIENTED_EDGE('',*,*,#3869,.T.);
#5227=ORIENTED_EDGE('',*,*,#3868,.F.);
#5228=ORIENTED_EDGE('',*,*,#3870,.F.);
#5229=ORIENTED_EDGE('',*,*,#3871,.T.);
#5230=ORIENTED_EDGE('',*,*,#3872,.T.);
#5231=ORIENTED_EDGE('',*,*,#3871,.F.);
#5232=ORIENTED_EDGE('',*,*,#3870,.T.);
#5233=ORIENTED_EDGE('',*,*,#3867,.T.);
#5234=ORIENTED_EDGE('',*,*,#3872,.F.);
#5235=ORIENTED_EDGE('',*,*,#3869,.F.);
#5236=ORIENTED_EDGE('',*,*,#3873,.F.);
#5237=ORIENTED_EDGE('',*,*,#3874,.F.);
#5238=ORIENTED_EDGE('',*,*,#3875,.T.);
#5239=ORIENTED_EDGE('',*,*,#3876,.T.);
#5240=ORIENTED_EDGE('',*,*,#3877,.F.);
#5241=ORIENTED_EDGE('',*,*,#3878,.F.);
#5242=ORIENTED_EDGE('',*,*,#3879,.T.);
#5243=ORIENTED_EDGE('',*,*,#3880,.T.);
#5244=ORIENTED_EDGE('',*,*,#3875,.F.);
#5245=ORIENTED_EDGE('',*,*,#3881,.F.);
#5246=ORIENTED_EDGE('',*,*,#3882,.T.);
#5247=ORIENTED_EDGE('',*,*,#3883,.T.);
#5248=ORIENTED_EDGE('',*,*,#3879,.F.);
#5249=ORIENTED_EDGE('',*,*,#3884,.F.);
#5250=ORIENTED_EDGE('',*,*,#3885,.T.);
#5251=ORIENTED_EDGE('',*,*,#3886,.T.);
#5252=ORIENTED_EDGE('',*,*,#3882,.F.);
#5253=ORIENTED_EDGE('',*,*,#3887,.F.);
#5254=ORIENTED_EDGE('',*,*,#3888,.T.);
#5255=ORIENTED_EDGE('',*,*,#3889,.T.);
#5256=ORIENTED_EDGE('',*,*,#3885,.F.);
#5257=ORIENTED_EDGE('',*,*,#3890,.F.);
#5258=ORIENTED_EDGE('',*,*,#3877,.T.);
#5259=ORIENTED_EDGE('',*,*,#3891,.T.);
#5260=ORIENTED_EDGE('',*,*,#3888,.F.);
#5261=ORIENTED_EDGE('',*,*,#3891,.F.);
#5262=ORIENTED_EDGE('',*,*,#3876,.F.);
#5263=ORIENTED_EDGE('',*,*,#3880,.F.);
#5264=ORIENTED_EDGE('',*,*,#3883,.F.);
#5265=ORIENTED_EDGE('',*,*,#3886,.F.);
#5266=ORIENTED_EDGE('',*,*,#3889,.F.);
#5267=ORIENTED_EDGE('',*,*,#3892,.F.);
#5268=ORIENTED_EDGE('',*,*,#3874,.T.);
#5269=ORIENTED_EDGE('',*,*,#3890,.T.);
#5270=ORIENTED_EDGE('',*,*,#3887,.T.);
#5271=ORIENTED_EDGE('',*,*,#3884,.T.);
#5272=ORIENTED_EDGE('',*,*,#3881,.T.);
#5273=ORIENTED_EDGE('',*,*,#3878,.T.);
#5274=ORIENTED_EDGE('',*,*,#3893,.F.);
#5275=ORIENTED_EDGE('',*,*,#3894,.T.);
#5276=ORIENTED_EDGE('',*,*,#3892,.T.);
#5277=ORIENTED_EDGE('',*,*,#3894,.F.);
#5278=ORIENTED_EDGE('',*,*,#3873,.T.);
#5279=ORIENTED_EDGE('',*,*,#3895,.T.);
#5280=ORIENTED_EDGE('',*,*,#3893,.T.);
#5281=ORIENTED_EDGE('',*,*,#3895,.F.);
#5282=ORIENTED_EDGE('',*,*,#3896,.F.);
#5283=ORIENTED_EDGE('',*,*,#3897,.F.);
#5284=ORIENTED_EDGE('',*,*,#3898,.F.);
#5285=ORIENTED_EDGE('',*,*,#3899,.T.);
#5286=ORIENTED_EDGE('',*,*,#3900,.F.);
#5287=ORIENTED_EDGE('',*,*,#3901,.F.);
#5288=ORIENTED_EDGE('',*,*,#3902,.F.);
#5289=ORIENTED_EDGE('',*,*,#3903,.F.);
#5290=ORIENTED_EDGE('',*,*,#3899,.F.);
#5291=ORIENTED_EDGE('',*,*,#3904,.F.);
#5292=ORIENTED_EDGE('',*,*,#3905,.F.);
#5293=ORIENTED_EDGE('',*,*,#3906,.T.);
#5294=ORIENTED_EDGE('',*,*,#3907,.F.);
#5295=ORIENTED_EDGE('',*,*,#3908,.F.);
#5296=ORIENTED_EDGE('',*,*,#3909,.F.);
#5297=ORIENTED_EDGE('',*,*,#3906,.F.);
#5298=ORIENTED_EDGE('',*,*,#3910,.F.);
#5299=ORIENTED_EDGE('',*,*,#3911,.T.);
#5300=ORIENTED_EDGE('',*,*,#3897,.T.);
#5301=ORIENTED_EDGE('',*,*,#3912,.T.);
#5302=ORIENTED_EDGE('',*,*,#3913,.F.);
#5303=ORIENTED_EDGE('',*,*,#3912,.F.);
#5304=ORIENTED_EDGE('',*,*,#3896,.T.);
#5305=ORIENTED_EDGE('',*,*,#3898,.T.);
#5306=ORIENTED_EDGE('',*,*,#3911,.F.);
#5307=ORIENTED_EDGE('',*,*,#3908,.T.);
#5308=ORIENTED_EDGE('',*,*,#3907,.T.);
#5309=ORIENTED_EDGE('',*,*,#3909,.T.);
#5310=ORIENTED_EDGE('',*,*,#3914,.T.);
#5311=ORIENTED_EDGE('',*,*,#3915,.T.);
#5312=ORIENTED_EDGE('',*,*,#3916,.T.);
#5313=ORIENTED_EDGE('',*,*,#3917,.T.);
#5314=ORIENTED_EDGE('',*,*,#3918,.T.);
#5315=ORIENTED_EDGE('',*,*,#3919,.T.);
#5316=ORIENTED_EDGE('',*,*,#3915,.F.);
#5317=ORIENTED_EDGE('',*,*,#3914,.F.);
#5318=ORIENTED_EDGE('',*,*,#3916,.F.);
#5319=ORIENTED_EDGE('',*,*,#3920,.T.);
#5320=ORIENTED_EDGE('',*,*,#3921,.F.);
#5321=ORIENTED_EDGE('',*,*,#3922,.F.);
#5322=ORIENTED_EDGE('',*,*,#3920,.F.);
#5323=ORIENTED_EDGE('',*,*,#3923,.F.);
#5324=ORIENTED_EDGE('',*,*,#3924,.F.);
#5325=ORIENTED_EDGE('',*,*,#3925,.T.);
#5326=ORIENTED_EDGE('',*,*,#3918,.F.);
#5327=ORIENTED_EDGE('',*,*,#3917,.F.);
#5328=ORIENTED_EDGE('',*,*,#3919,.F.);
#5329=ORIENTED_EDGE('',*,*,#3925,.F.);
#5330=ORIENTED_EDGE('',*,*,#3926,.F.);
#5331=ORIENTED_EDGE('',*,*,#3927,.T.);
#5332=ORIENTED_EDGE('',*,*,#3900,.T.);
#5333=ORIENTED_EDGE('',*,*,#3903,.T.);
#5334=ORIENTED_EDGE('',*,*,#3928,.T.);
#5335=ORIENTED_EDGE('',*,*,#3929,.F.);
#5336=ORIENTED_EDGE('',*,*,#3928,.F.);
#5337=ORIENTED_EDGE('',*,*,#3902,.T.);
#5338=ORIENTED_EDGE('',*,*,#3901,.T.);
#5339=ORIENTED_EDGE('',*,*,#3927,.F.);
#5340=ORIENTED_EDGE('',*,*,#3904,.T.);
#5341=ORIENTED_EDGE('',*,*,#3905,.T.);
#5342=ORIENTED_EDGE('',*,*,#3923,.T.);
#5343=ORIENTED_EDGE('',*,*,#3924,.T.);
#5344=ORIENTED_EDGE('',*,*,#3921,.T.);
#5345=ORIENTED_EDGE('',*,*,#3922,.T.);
#5346=ORIENTED_EDGE('',*,*,#3910,.T.);
#5347=ORIENTED_EDGE('',*,*,#3926,.T.);
#5348=ORIENTED_EDGE('',*,*,#3930,.T.);
#5349=ORIENTED_EDGE('',*,*,#3931,.T.);
#5350=ORIENTED_EDGE('',*,*,#3932,.F.);
#5351=ORIENTED_EDGE('',*,*,#3933,.T.);
#5352=ORIENTED_EDGE('',*,*,#3934,.F.);
#5353=ORIENTED_EDGE('',*,*,#3935,.T.);
#5354=ORIENTED_EDGE('',*,*,#3936,.F.);
#5355=ORIENTED_EDGE('',*,*,#3937,.T.);
#5356=ORIENTED_EDGE('',*,*,#3938,.F.);
#5357=ORIENTED_EDGE('',*,*,#3939,.T.);
#5358=ORIENTED_EDGE('',*,*,#3940,.F.);
#5359=ORIENTED_EDGE('',*,*,#3941,.T.);
#5360=ORIENTED_EDGE('',*,*,#3942,.F.);
#5361=ORIENTED_EDGE('',*,*,#3943,.T.);
#5362=ORIENTED_EDGE('',*,*,#3944,.F.);
#5363=ORIENTED_EDGE('',*,*,#3945,.T.);
#5364=ORIENTED_EDGE('',*,*,#3946,.F.);
#5365=ORIENTED_EDGE('',*,*,#3947,.T.);
#5366=ORIENTED_EDGE('',*,*,#3948,.F.);
#5367=ORIENTED_EDGE('',*,*,#3949,.T.);
#5368=ORIENTED_EDGE('',*,*,#3950,.F.);
#5369=ORIENTED_EDGE('',*,*,#3951,.T.);
#5370=ORIENTED_EDGE('',*,*,#3952,.F.);
#5371=ORIENTED_EDGE('',*,*,#3953,.T.);
#5372=ORIENTED_EDGE('',*,*,#3954,.F.);
#5373=ORIENTED_EDGE('',*,*,#3955,.T.);
#5374=ORIENTED_EDGE('',*,*,#3956,.F.);
#5375=ORIENTED_EDGE('',*,*,#3957,.T.);
#5376=ORIENTED_EDGE('',*,*,#3958,.F.);
#5377=ORIENTED_EDGE('',*,*,#3959,.T.);
#5378=ORIENTED_EDGE('',*,*,#3960,.F.);
#5379=ORIENTED_EDGE('',*,*,#3961,.T.);
#5380=ORIENTED_EDGE('',*,*,#3962,.F.);
#5381=ORIENTED_EDGE('',*,*,#3963,.T.);
#5382=ORIENTED_EDGE('',*,*,#3964,.F.);
#5383=ORIENTED_EDGE('',*,*,#3965,.T.);
#5384=ORIENTED_EDGE('',*,*,#3966,.F.);
#5385=ORIENTED_EDGE('',*,*,#3967,.T.);
#5386=ORIENTED_EDGE('',*,*,#3968,.F.);
#5387=ORIENTED_EDGE('',*,*,#3969,.T.);
#5388=ORIENTED_EDGE('',*,*,#3970,.F.);
#5389=ORIENTED_EDGE('',*,*,#3971,.F.);
#5390=ORIENTED_EDGE('',*,*,#3972,.T.);
#5391=ORIENTED_EDGE('',*,*,#3930,.F.);
#5392=ORIENTED_EDGE('',*,*,#3972,.F.);
#5393=ORIENTED_EDGE('',*,*,#3971,.T.);
#5394=ORIENTED_EDGE('',*,*,#3913,.T.);
#5395=ORIENTED_EDGE('',*,*,#3973,.F.);
#5396=ORIENTED_EDGE('',*,*,#3974,.T.);
#5397=ORIENTED_EDGE('',*,*,#3975,.T.);
#5398=ORIENTED_EDGE('',*,*,#3976,.T.);
#5399=ORIENTED_EDGE('',*,*,#3977,.T.);
#5400=ORIENTED_EDGE('',*,*,#3978,.T.);
#5401=ORIENTED_EDGE('',*,*,#3979,.T.);
#5402=ORIENTED_EDGE('',*,*,#3980,.T.);
#5403=ORIENTED_EDGE('',*,*,#3981,.T.);
#5404=ORIENTED_EDGE('',*,*,#3982,.T.);
#5405=ORIENTED_EDGE('',*,*,#3983,.T.);
#5406=ORIENTED_EDGE('',*,*,#3984,.T.);
#5407=ORIENTED_EDGE('',*,*,#3985,.T.);
#5408=ORIENTED_EDGE('',*,*,#3986,.T.);
#5409=ORIENTED_EDGE('',*,*,#3987,.T.);
#5410=ORIENTED_EDGE('',*,*,#3988,.T.);
#5411=ORIENTED_EDGE('',*,*,#3989,.T.);
#5412=ORIENTED_EDGE('',*,*,#3990,.T.);
#5413=ORIENTED_EDGE('',*,*,#3991,.T.);
#5414=ORIENTED_EDGE('',*,*,#3992,.T.);
#5415=ORIENTED_EDGE('',*,*,#3993,.T.);
#5416=ORIENTED_EDGE('',*,*,#3994,.T.);
#5417=ORIENTED_EDGE('',*,*,#3995,.T.);
#5418=ORIENTED_EDGE('',*,*,#3996,.T.);
#5419=ORIENTED_EDGE('',*,*,#3997,.T.);
#5420=ORIENTED_EDGE('',*,*,#3998,.T.);
#5421=ORIENTED_EDGE('',*,*,#3999,.T.);
#5422=ORIENTED_EDGE('',*,*,#4000,.T.);
#5423=ORIENTED_EDGE('',*,*,#4001,.T.);
#5424=ORIENTED_EDGE('',*,*,#4002,.T.);
#5425=ORIENTED_EDGE('',*,*,#4003,.T.);
#5426=ORIENTED_EDGE('',*,*,#4004,.T.);
#5427=ORIENTED_EDGE('',*,*,#4005,.T.);
#5428=ORIENTED_EDGE('',*,*,#4006,.T.);
#5429=ORIENTED_EDGE('',*,*,#4007,.T.);
#5430=ORIENTED_EDGE('',*,*,#4008,.T.);
#5431=ORIENTED_EDGE('',*,*,#4009,.T.);
#5432=ORIENTED_EDGE('',*,*,#4010,.T.);
#5433=ORIENTED_EDGE('',*,*,#4011,.T.);
#5434=ORIENTED_EDGE('',*,*,#4012,.T.);
#5435=ORIENTED_EDGE('',*,*,#4013,.T.);
#5436=ORIENTED_EDGE('',*,*,#4014,.F.);
#5437=ORIENTED_EDGE('',*,*,#4015,.T.);
#5438=ORIENTED_EDGE('',*,*,#3973,.T.);
#5439=ORIENTED_EDGE('',*,*,#4015,.F.);
#5440=ORIENTED_EDGE('',*,*,#4014,.T.);
#5441=ORIENTED_EDGE('',*,*,#3929,.T.);
#5442=ORIENTED_EDGE('',*,*,#4016,.F.);
#5443=ORIENTED_EDGE('',*,*,#3974,.F.);
#5444=ORIENTED_EDGE('',*,*,#4017,.F.);
#5445=ORIENTED_EDGE('',*,*,#3931,.F.);
#5446=ORIENTED_EDGE('',*,*,#4017,.T.);
#5447=ORIENTED_EDGE('',*,*,#4013,.F.);
#5448=ORIENTED_EDGE('',*,*,#4018,.T.);
#5449=ORIENTED_EDGE('',*,*,#3932,.T.);
#5450=ORIENTED_EDGE('',*,*,#4018,.F.);
#5451=ORIENTED_EDGE('',*,*,#4012,.F.);
#5452=ORIENTED_EDGE('',*,*,#4019,.F.);
#5453=ORIENTED_EDGE('',*,*,#3933,.F.);
#5454=ORIENTED_EDGE('',*,*,#4019,.T.);
#5455=ORIENTED_EDGE('',*,*,#4011,.F.);
#5456=ORIENTED_EDGE('',*,*,#4020,.T.);
#5457=ORIENTED_EDGE('',*,*,#3934,.T.);
#5458=ORIENTED_EDGE('',*,*,#4020,.F.);
#5459=ORIENTED_EDGE('',*,*,#4010,.F.);
#5460=ORIENTED_EDGE('',*,*,#4021,.F.);
#5461=ORIENTED_EDGE('',*,*,#3935,.F.);
#5462=ORIENTED_EDGE('',*,*,#4021,.T.);
#5463=ORIENTED_EDGE('',*,*,#4009,.F.);
#5464=ORIENTED_EDGE('',*,*,#4022,.T.);
#5465=ORIENTED_EDGE('',*,*,#3936,.T.);
#5466=ORIENTED_EDGE('',*,*,#4022,.F.);
#5467=ORIENTED_EDGE('',*,*,#4008,.F.);
#5468=ORIENTED_EDGE('',*,*,#4023,.F.);
#5469=ORIENTED_EDGE('',*,*,#3937,.F.);
#5470=ORIENTED_EDGE('',*,*,#4023,.T.);
#5471=ORIENTED_EDGE('',*,*,#4007,.F.);
#5472=ORIENTED_EDGE('',*,*,#4024,.T.);
#5473=ORIENTED_EDGE('',*,*,#3938,.T.);
#5474=ORIENTED_EDGE('',*,*,#4024,.F.);
#5475=ORIENTED_EDGE('',*,*,#4006,.F.);
#5476=ORIENTED_EDGE('',*,*,#4025,.F.);
#5477=ORIENTED_EDGE('',*,*,#3939,.F.);
#5478=ORIENTED_EDGE('',*,*,#4025,.T.);
#5479=ORIENTED_EDGE('',*,*,#4005,.F.);
#5480=ORIENTED_EDGE('',*,*,#4026,.T.);
#5481=ORIENTED_EDGE('',*,*,#3940,.T.);
#5482=ORIENTED_EDGE('',*,*,#4026,.F.);
#5483=ORIENTED_EDGE('',*,*,#4004,.F.);
#5484=ORIENTED_EDGE('',*,*,#4027,.F.);
#5485=ORIENTED_EDGE('',*,*,#3941,.F.);
#5486=ORIENTED_EDGE('',*,*,#4027,.T.);
#5487=ORIENTED_EDGE('',*,*,#4003,.F.);
#5488=ORIENTED_EDGE('',*,*,#4028,.T.);
#5489=ORIENTED_EDGE('',*,*,#3942,.T.);
#5490=ORIENTED_EDGE('',*,*,#4028,.F.);
#5491=ORIENTED_EDGE('',*,*,#4002,.F.);
#5492=ORIENTED_EDGE('',*,*,#4029,.F.);
#5493=ORIENTED_EDGE('',*,*,#3943,.F.);
#5494=ORIENTED_EDGE('',*,*,#4029,.T.);
#5495=ORIENTED_EDGE('',*,*,#4001,.F.);
#5496=ORIENTED_EDGE('',*,*,#4030,.T.);
#5497=ORIENTED_EDGE('',*,*,#3944,.T.);
#5498=ORIENTED_EDGE('',*,*,#4030,.F.);
#5499=ORIENTED_EDGE('',*,*,#4000,.F.);
#5500=ORIENTED_EDGE('',*,*,#4031,.F.);
#5501=ORIENTED_EDGE('',*,*,#3945,.F.);
#5502=ORIENTED_EDGE('',*,*,#4031,.T.);
#5503=ORIENTED_EDGE('',*,*,#3999,.F.);
#5504=ORIENTED_EDGE('',*,*,#4032,.T.);
#5505=ORIENTED_EDGE('',*,*,#3946,.T.);
#5506=ORIENTED_EDGE('',*,*,#4032,.F.);
#5507=ORIENTED_EDGE('',*,*,#3998,.F.);
#5508=ORIENTED_EDGE('',*,*,#4033,.F.);
#5509=ORIENTED_EDGE('',*,*,#3947,.F.);
#5510=ORIENTED_EDGE('',*,*,#4033,.T.);
#5511=ORIENTED_EDGE('',*,*,#3997,.F.);
#5512=ORIENTED_EDGE('',*,*,#4034,.T.);
#5513=ORIENTED_EDGE('',*,*,#3948,.T.);
#5514=ORIENTED_EDGE('',*,*,#4034,.F.);
#5515=ORIENTED_EDGE('',*,*,#3996,.F.);
#5516=ORIENTED_EDGE('',*,*,#4035,.F.);
#5517=ORIENTED_EDGE('',*,*,#3949,.F.);
#5518=ORIENTED_EDGE('',*,*,#4035,.T.);
#5519=ORIENTED_EDGE('',*,*,#3995,.F.);
#5520=ORIENTED_EDGE('',*,*,#4036,.T.);
#5521=ORIENTED_EDGE('',*,*,#3950,.T.);
#5522=ORIENTED_EDGE('',*,*,#4036,.F.);
#5523=ORIENTED_EDGE('',*,*,#3994,.F.);
#5524=ORIENTED_EDGE('',*,*,#4037,.F.);
#5525=ORIENTED_EDGE('',*,*,#3951,.F.);
#5526=ORIENTED_EDGE('',*,*,#4037,.T.);
#5527=ORIENTED_EDGE('',*,*,#3993,.F.);
#5528=ORIENTED_EDGE('',*,*,#4038,.T.);
#5529=ORIENTED_EDGE('',*,*,#3952,.T.);
#5530=ORIENTED_EDGE('',*,*,#4038,.F.);
#5531=ORIENTED_EDGE('',*,*,#3992,.F.);
#5532=ORIENTED_EDGE('',*,*,#4039,.F.);
#5533=ORIENTED_EDGE('',*,*,#3953,.F.);
#5534=ORIENTED_EDGE('',*,*,#4039,.T.);
#5535=ORIENTED_EDGE('',*,*,#3991,.F.);
#5536=ORIENTED_EDGE('',*,*,#4040,.T.);
#5537=ORIENTED_EDGE('',*,*,#3954,.T.);
#5538=ORIENTED_EDGE('',*,*,#4040,.F.);
#5539=ORIENTED_EDGE('',*,*,#3990,.F.);
#5540=ORIENTED_EDGE('',*,*,#4041,.F.);
#5541=ORIENTED_EDGE('',*,*,#3955,.F.);
#5542=ORIENTED_EDGE('',*,*,#4041,.T.);
#5543=ORIENTED_EDGE('',*,*,#3989,.F.);
#5544=ORIENTED_EDGE('',*,*,#4042,.T.);
#5545=ORIENTED_EDGE('',*,*,#3956,.T.);
#5546=ORIENTED_EDGE('',*,*,#4042,.F.);
#5547=ORIENTED_EDGE('',*,*,#3988,.F.);
#5548=ORIENTED_EDGE('',*,*,#4043,.F.);
#5549=ORIENTED_EDGE('',*,*,#3957,.F.);
#5550=ORIENTED_EDGE('',*,*,#4043,.T.);
#5551=ORIENTED_EDGE('',*,*,#3987,.F.);
#5552=ORIENTED_EDGE('',*,*,#4044,.T.);
#5553=ORIENTED_EDGE('',*,*,#3958,.T.);
#5554=ORIENTED_EDGE('',*,*,#4044,.F.);
#5555=ORIENTED_EDGE('',*,*,#3986,.F.);
#5556=ORIENTED_EDGE('',*,*,#4045,.F.);
#5557=ORIENTED_EDGE('',*,*,#3959,.F.);
#5558=ORIENTED_EDGE('',*,*,#4045,.T.);
#5559=ORIENTED_EDGE('',*,*,#3985,.F.);
#5560=ORIENTED_EDGE('',*,*,#4046,.T.);
#5561=ORIENTED_EDGE('',*,*,#3960,.T.);
#5562=ORIENTED_EDGE('',*,*,#4046,.F.);
#5563=ORIENTED_EDGE('',*,*,#3984,.F.);
#5564=ORIENTED_EDGE('',*,*,#4047,.F.);
#5565=ORIENTED_EDGE('',*,*,#3961,.F.);
#5566=ORIENTED_EDGE('',*,*,#4047,.T.);
#5567=ORIENTED_EDGE('',*,*,#3983,.F.);
#5568=ORIENTED_EDGE('',*,*,#4048,.T.);
#5569=ORIENTED_EDGE('',*,*,#3962,.T.);
#5570=ORIENTED_EDGE('',*,*,#4048,.F.);
#5571=ORIENTED_EDGE('',*,*,#3982,.F.);
#5572=ORIENTED_EDGE('',*,*,#4049,.F.);
#5573=ORIENTED_EDGE('',*,*,#3963,.F.);
#5574=ORIENTED_EDGE('',*,*,#4049,.T.);
#5575=ORIENTED_EDGE('',*,*,#3981,.F.);
#5576=ORIENTED_EDGE('',*,*,#4050,.T.);
#5577=ORIENTED_EDGE('',*,*,#3964,.T.);
#5578=ORIENTED_EDGE('',*,*,#4050,.F.);
#5579=ORIENTED_EDGE('',*,*,#3980,.F.);
#5580=ORIENTED_EDGE('',*,*,#4051,.F.);
#5581=ORIENTED_EDGE('',*,*,#3965,.F.);
#5582=ORIENTED_EDGE('',*,*,#4051,.T.);
#5583=ORIENTED_EDGE('',*,*,#3979,.F.);
#5584=ORIENTED_EDGE('',*,*,#4052,.T.);
#5585=ORIENTED_EDGE('',*,*,#3966,.T.);
#5586=ORIENTED_EDGE('',*,*,#4053,.F.);
#5587=ORIENTED_EDGE('',*,*,#3967,.F.);
#5588=ORIENTED_EDGE('',*,*,#4052,.F.);
#5589=ORIENTED_EDGE('',*,*,#3978,.F.);
#5590=ORIENTED_EDGE('',*,*,#4016,.T.);
#5591=ORIENTED_EDGE('',*,*,#3970,.T.);
#5592=ORIENTED_EDGE('',*,*,#4054,.T.);
#5593=ORIENTED_EDGE('',*,*,#3975,.F.);
#5594=ORIENTED_EDGE('',*,*,#4055,.F.);
#5595=ORIENTED_EDGE('',*,*,#3976,.F.);
#5596=ORIENTED_EDGE('',*,*,#4054,.F.);
#5597=ORIENTED_EDGE('',*,*,#3969,.F.);
#5598=ORIENTED_EDGE('',*,*,#4053,.T.);
#5599=ORIENTED_EDGE('',*,*,#3977,.F.);
#5600=ORIENTED_EDGE('',*,*,#4055,.T.);
#5601=ORIENTED_EDGE('',*,*,#3968,.T.);
#5602=ORIENTED_EDGE('',*,*,#4056,.T.);
#5603=ORIENTED_EDGE('',*,*,#4057,.T.);
#5604=ORIENTED_EDGE('',*,*,#4058,.T.);
#5605=ORIENTED_EDGE('',*,*,#4059,.F.);
#5606=ORIENTED_EDGE('',*,*,#4060,.T.);
#5607=ORIENTED_EDGE('',*,*,#4061,.T.);
#5608=ORIENTED_EDGE('',*,*,#4062,.T.);
#5609=ORIENTED_EDGE('',*,*,#4057,.F.);
#5610=ORIENTED_EDGE('',*,*,#4063,.T.);
#5611=ORIENTED_EDGE('',*,*,#4064,.T.);
#5612=ORIENTED_EDGE('',*,*,#4065,.T.);
#5613=ORIENTED_EDGE('',*,*,#4061,.F.);
#5614=ORIENTED_EDGE('',*,*,#4066,.T.);
#5615=ORIENTED_EDGE('',*,*,#4067,.T.);
#5616=ORIENTED_EDGE('',*,*,#4068,.T.);
#5617=ORIENTED_EDGE('',*,*,#4064,.F.);
#5618=ORIENTED_EDGE('',*,*,#4069,.T.);
#5619=ORIENTED_EDGE('',*,*,#4070,.T.);
#5620=ORIENTED_EDGE('',*,*,#4071,.T.);
#5621=ORIENTED_EDGE('',*,*,#4067,.F.);
#5622=ORIENTED_EDGE('',*,*,#4072,.T.);
#5623=ORIENTED_EDGE('',*,*,#4059,.T.);
#5624=ORIENTED_EDGE('',*,*,#4073,.T.);
#5625=ORIENTED_EDGE('',*,*,#4070,.F.);
#5626=ORIENTED_EDGE('',*,*,#4072,.F.);
#5627=ORIENTED_EDGE('',*,*,#4069,.F.);
#5628=ORIENTED_EDGE('',*,*,#4066,.F.);
#5629=ORIENTED_EDGE('',*,*,#4063,.F.);
#5630=ORIENTED_EDGE('',*,*,#4060,.F.);
#5631=ORIENTED_EDGE('',*,*,#4056,.F.);
#5632=ORIENTED_EDGE('',*,*,#4073,.F.);
#5633=ORIENTED_EDGE('',*,*,#4058,.F.);
#5634=ORIENTED_EDGE('',*,*,#4062,.F.);
#5635=ORIENTED_EDGE('',*,*,#4065,.F.);
#5636=ORIENTED_EDGE('',*,*,#4068,.F.);
#5637=ORIENTED_EDGE('',*,*,#4071,.F.);
#5638=ORIENTED_EDGE('',*,*,#4074,.F.);
#5639=ORIENTED_EDGE('',*,*,#4075,.F.);
#5640=ORIENTED_EDGE('',*,*,#4076,.F.);
#5641=ORIENTED_EDGE('',*,*,#4077,.T.);
#5642=ORIENTED_EDGE('',*,*,#4075,.T.);
#5643=ORIENTED_EDGE('',*,*,#4077,.F.);
#5644=ORIENTED_EDGE('',*,*,#4078,.F.);
#5645=ORIENTED_EDGE('',*,*,#4079,.T.);
#5646=ORIENTED_EDGE('',*,*,#4076,.T.);
#5647=ORIENTED_EDGE('',*,*,#4079,.F.);
#5648=ORIENTED_EDGE('',*,*,#4080,.F.);
#5649=ORIENTED_EDGE('',*,*,#4081,.T.);
#5650=ORIENTED_EDGE('',*,*,#4078,.T.);
#5651=ORIENTED_EDGE('',*,*,#4081,.F.);
#5652=ORIENTED_EDGE('',*,*,#4080,.T.);
#5653=ORIENTED_EDGE('',*,*,#4082,.F.);
#5654=ORIENTED_EDGE('',*,*,#4083,.F.);
#5655=ORIENTED_EDGE('',*,*,#4084,.T.);
#5656=ORIENTED_EDGE('',*,*,#4082,.T.);
#5657=ORIENTED_EDGE('',*,*,#4084,.F.);
#5658=ORIENTED_EDGE('',*,*,#4074,.T.);
#5659=ORIENTED_EDGE('',*,*,#4085,.T.);
#5660=ORIENTED_EDGE('',*,*,#4083,.T.);
#5661=ORIENTED_EDGE('',*,*,#4085,.F.);
#5662=CYLINDRICAL_SURFACE('',#6605,0.225);
#5663=CYLINDRICAL_SURFACE('',#6608,0.225);
#5664=CYLINDRICAL_SURFACE('',#6611,0.21);
#5665=CYLINDRICAL_SURFACE('',#6614,0.21);
#5666=CYLINDRICAL_SURFACE('',#6617,0.21);
#5667=CYLINDRICAL_SURFACE('',#6641,0.275);
#5668=CYLINDRICAL_SURFACE('',#6644,0.275);
#5669=CYLINDRICAL_SURFACE('',#6647,0.275);
#5670=CYLINDRICAL_SURFACE('',#6653,0.7);
#5671=CYLINDRICAL_SURFACE('',#6655,0.5);
#5672=CYLINDRICAL_SURFACE('',#6661,2.8);
#5673=CYLINDRICAL_SURFACE('',#6663,1.2);
#5674=CYLINDRICAL_SURFACE('',#6670,0.165);
#5675=CYLINDRICAL_SURFACE('',#6673,0.505);
#5676=CYLINDRICAL_SURFACE('',#6676,0.9);
#5677=CYLINDRICAL_SURFACE('',#6682,0.165);
#5678=CYLINDRICAL_SURFACE('',#6686,0.07);
#5679=CYLINDRICAL_SURFACE('',#6687,0.5);
#5680=CYLINDRICAL_SURFACE('',#6693,0.0599999999999996);
#5681=CYLINDRICAL_SURFACE('',#6702,0.0600000000000001);
#5682=CYLINDRICAL_SURFACE('',#6709,0.0600000000000001);
#5683=CYLINDRICAL_SURFACE('',#6716,0.165);
#5684=CYLINDRICAL_SURFACE('',#6720,0.21);
#5685=CYLINDRICAL_SURFACE('',#6733,0.265);
#5686=CYLINDRICAL_SURFACE('',#6737,0.5);
#5687=CYLINDRICAL_SURFACE('',#6745,0.425);
#5688=CYLINDRICAL_SURFACE('',#6753,0.24505);
#5689=CYLINDRICAL_SURFACE('',#6774,0.2117);
#5690=CYLINDRICAL_SURFACE('',#6787,0.35);
#5691=CYLINDRICAL_SURFACE('',#6795,0.1954);
#5692=CYLINDRICAL_SURFACE('',#6810,0.165);
#5693=CYLINDRICAL_SURFACE('',#6813,0.165);
#5694=CYLINDRICAL_SURFACE('',#6816,0.164999999999999);
#5695=CYLINDRICAL_SURFACE('',#6819,0.164999999999999);
#5696=CYLINDRICAL_SURFACE('',#6822,0.165);
#5697=CYLINDRICAL_SURFACE('',#6825,0.165);
#5698=CYLINDRICAL_SURFACE('',#6828,0.165);
#5699=CYLINDRICAL_SURFACE('',#6831,0.165);
#5700=CYLINDRICAL_SURFACE('',#6834,1.5);
#5701=CYLINDRICAL_SURFACE('',#6837,1.5);
#5702=CYLINDRICAL_SURFACE('',#6840,2.);
#5703=CYLINDRICAL_SURFACE('',#6847,2.);
#5704=CYLINDRICAL_SURFACE('',#6851,0.225);
#5705=CYLINDRICAL_SURFACE('',#6854,0.225);
#5706=CYLINDRICAL_SURFACE('',#6857,0.225);
#5707=CYLINDRICAL_SURFACE('',#6860,0.225);
#5708=CYLINDRICAL_SURFACE('',#6863,1.49);
#5709=CYLINDRICAL_SURFACE('',#6868,1.02);
#5710=CYLINDRICAL_SURFACE('',#6870,2.);
#5711=CYLINDRICAL_SURFACE('',#6876,0.225);
#5712=CYLINDRICAL_SURFACE('',#6879,0.225);
#5713=CYLINDRICAL_SURFACE('',#6882,0.225);
#5714=CYLINDRICAL_SURFACE('',#6885,0.225);
#5715=CYLINDRICAL_SURFACE('',#6888,1.49);
#5716=CYLINDRICAL_SURFACE('',#6893,1.02);
#5717=CYLINDRICAL_SURFACE('',#6895,2.);
#5718=CYLINDRICAL_SURFACE('',#6901,0.225);
#5719=CYLINDRICAL_SURFACE('',#6904,0.225);
#5720=CYLINDRICAL_SURFACE('',#6907,0.225);
#5721=CYLINDRICAL_SURFACE('',#6910,0.225);
#5722=CYLINDRICAL_SURFACE('',#6913,1.49);
#5723=CYLINDRICAL_SURFACE('',#6918,1.02);
#5724=CYLINDRICAL_SURFACE('',#6920,2.);
#5725=CYLINDRICAL_SURFACE('',#6926,0.225);
#5726=CYLINDRICAL_SURFACE('',#6929,0.225);
#5727=CYLINDRICAL_SURFACE('',#6932,0.225);
#5728=CYLINDRICAL_SURFACE('',#6935,0.225);
#5729=CYLINDRICAL_SURFACE('',#6938,1.49);
#5730=CYLINDRICAL_SURFACE('',#6943,1.02);
#5731=CYLINDRICAL_SURFACE('',#6945,2.);
#5732=CYLINDRICAL_SURFACE('',#6951,0.0700000000000003);
#5733=CYLINDRICAL_SURFACE('',#6952,0.5);
#5734=CYLINDRICAL_SURFACE('',#6974,0.976185);
#5735=CYLINDRICAL_SURFACE('',#6976,0.5);
#5736=CYLINDRICAL_SURFACE('',#6982,0.976185);
#5737=CYLINDRICAL_SURFACE('',#6994,1.023815);
#5738=CYLINDRICAL_SURFACE('',#7001,1.5);
#5739=CYLINDRICAL_SURFACE('',#7006,1.023815);
#5740=CYLINDRICAL_SURFACE('',#7028,1.019052);
#5741=CYLINDRICAL_SURFACE('',#7068,0.980948);
#5742=CYLINDRICAL_SURFACE('',#7082,1.013815);
#5743=CYLINDRICAL_SURFACE('',#7086,0.991185);
#5744=CYLINDRICAL_SURFACE('',#7090,1.013815);
#5745=CYLINDRICAL_SURFACE('',#7094,0.991185);
#5746=CYLINDRICAL_SURFACE('',#7107,0.35);
#5747=CYLINDRICAL_SURFACE('',#7115,0.1954);
#5748=CYLINDRICAL_SURFACE('',#7150,0.164999999999999);
#5749=CYLINDRICAL_SURFACE('',#7154,0.4);
#5750=CYLINDRICAL_SURFACE('',#7161,0.699999999999999);
#5751=CYLINDRICAL_SURFACE('',#7163,0.5);
#5752=CYLINDRICAL_SURFACE('',#7170,0.165);
#5753=CYLINDRICAL_SURFACE('',#7173,0.505000000000001);
#5754=CYLINDRICAL_SURFACE('',#7176,0.9);
#5755=CYLINDRICAL_SURFACE('',#7182,0.404999999999999);
#5756=CYLINDRICAL_SURFACE('',#7185,0.6);
#5757=CYLINDRICAL_SURFACE('',#7191,0.404999999999999);
#5758=CYLINDRICAL_SURFACE('',#7194,0.6);
#5759=CYLINDRICAL_SURFACE('',#7200,0.15);
#5760=CYLINDRICAL_SURFACE('',#7206,0.15);
#5761=CYLINDRICAL_SURFACE('',#7212,0.225);
#5762=CYLINDRICAL_SURFACE('',#7215,0.6);
#5763=CYLINDRICAL_SURFACE('',#7234,0.1954);
#5764=CYLINDRICAL_SURFACE('',#7255,0.125);
#5765=CYLINDRICAL_SURFACE('',#7256,0.125);
#5766=CYLINDRICAL_SURFACE('',#7257,0.65);
#5767=CYLINDRICAL_SURFACE('',#7260,0.125);
#5768=CYLINDRICAL_SURFACE('',#7261,0.125);
#5769=CYLINDRICAL_SURFACE('',#7262,0.4);
#5770=CYLINDRICAL_SURFACE('',#7308,0.8);
#5771=CYLINDRICAL_SURFACE('',#7353,0.8);
#5772=CYLINDRICAL_SURFACE('',#7356,0.0555);
#5773=CYLINDRICAL_SURFACE('',#7357,0.611219772367581);
#5774=CYLINDRICAL_SURFACE('',#7358,0.0555);
#5775=CYLINDRICAL_SURFACE('',#7359,0.611219772367581);
#5776=CYLINDRICAL_SURFACE('',#7360,0.0555);
#5777=CYLINDRICAL_SURFACE('',#7361,0.611219772367581);
#5778=CYLINDRICAL_SURFACE('',#7362,0.0555);
#5779=CYLINDRICAL_SURFACE('',#7363,0.611219772367581);
#5780=CYLINDRICAL_SURFACE('',#7364,0.0555);
#5781=CYLINDRICAL_SURFACE('',#7365,0.611219772367581);
#5782=CYLINDRICAL_SURFACE('',#7366,0.0555);
#5783=CYLINDRICAL_SURFACE('',#7367,0.611219772367581);
#5784=CYLINDRICAL_SURFACE('',#7368,0.0555);
#5785=CYLINDRICAL_SURFACE('',#7369,0.611219772367581);
#5786=CYLINDRICAL_SURFACE('',#7370,0.0555);
#5787=CYLINDRICAL_SURFACE('',#7371,0.611219772367581);
#5788=CYLINDRICAL_SURFACE('',#7372,0.0555);
#5789=CYLINDRICAL_SURFACE('',#7373,0.611219772367581);
#5790=CYLINDRICAL_SURFACE('',#7374,0.0555);
#5791=CYLINDRICAL_SURFACE('',#7375,0.611219772367581);
#5792=CYLINDRICAL_SURFACE('',#7376,0.0555);
#5793=CYLINDRICAL_SURFACE('',#7377,0.611219772367581);
#5794=CYLINDRICAL_SURFACE('',#7378,0.0555);
#5795=CYLINDRICAL_SURFACE('',#7379,0.611219772367581);
#5796=CYLINDRICAL_SURFACE('',#7380,0.0555);
#5797=CYLINDRICAL_SURFACE('',#7381,0.611219772367581);
#5798=CYLINDRICAL_SURFACE('',#7382,0.0555);
#5799=CYLINDRICAL_SURFACE('',#7383,0.611219772367581);
#5800=CYLINDRICAL_SURFACE('',#7384,0.0555);
#5801=CYLINDRICAL_SURFACE('',#7385,0.611219772367581);
#5802=CYLINDRICAL_SURFACE('',#7386,0.0555);
#5803=CYLINDRICAL_SURFACE('',#7387,0.611219772367581);
#5804=CYLINDRICAL_SURFACE('',#7388,0.0555);
#5805=CYLINDRICAL_SURFACE('',#7389,0.611219772367581);
#5806=CYLINDRICAL_SURFACE('',#7390,0.0555);
#5807=CYLINDRICAL_SURFACE('',#7391,0.611219772367581);
#5808=CYLINDRICAL_SURFACE('',#7392,0.0555);
#5809=CYLINDRICAL_SURFACE('',#7393,0.611219772367581);
#5810=CYLINDRICAL_SURFACE('',#7394,0.0555);
#5811=CYLINDRICAL_SURFACE('',#7395,0.611219772367581);
#5812=CYLINDRICAL_SURFACE('',#7411,0.35);
#5813=CYLINDRICAL_SURFACE('',#7419,0.1954);
#5814=ADVANCED_FACE('',(#837),#5662,.F.);
#5815=ADVANCED_FACE('',(#838),#5663,.F.);
#5816=ADVANCED_FACE('',(#839),#5664,.F.);
#5817=ADVANCED_FACE('',(#840),#5665,.F.);
#5818=ADVANCED_FACE('',(#841),#5666,.F.);
#5819=ADVANCED_FACE('',(#842),#663,.T.);
#5820=ADVANCED_FACE('',(#843),#664,.T.);
#5821=ADVANCED_FACE('',(#844),#665,.T.);
#5822=ADVANCED_FACE('',(#845),#666,.T.);
#5823=ADVANCED_FACE('',(#846,#527,#528,#529,#530,#531),#667,.T.);
#5824=ADVANCED_FACE('',(#847,#532,#533,#534,#535,#536),#668,.F.);
#5825=ADVANCED_FACE('',(#848),#669,.T.);
#5826=ADVANCED_FACE('',(#849),#670,.T.);
#5827=ADVANCED_FACE('',(#850),#671,.T.);
#5828=ADVANCED_FACE('',(#851),#672,.T.);
#5829=ADVANCED_FACE('',(#852),#673,.T.);
#5830=ADVANCED_FACE('',(#853),#674,.F.);
#5831=ADVANCED_FACE('',(#854),#675,.T.);
#5832=ADVANCED_FACE('',(#855),#676,.T.);
#5833=ADVANCED_FACE('',(#856),#677,.T.);
#5834=ADVANCED_FACE('',(#857),#678,.T.);
#5835=ADVANCED_FACE('',(#858),#679,.T.);
#5836=ADVANCED_FACE('',(#859),#680,.F.);
#5837=ADVANCED_FACE('',(#860),#5667,.F.);
#5838=ADVANCED_FACE('',(#861),#5668,.F.);
#5839=ADVANCED_FACE('',(#862),#5669,.F.);
#5840=ADVANCED_FACE('',(#863,#537),#681,.T.);
#5841=ADVANCED_FACE('',(#864),#5670,.T.);
#5842=ADVANCED_FACE('',(#865),#5671,.T.);
#5843=ADVANCED_FACE('',(#866),#682,.T.);
#5844=ADVANCED_FACE('',(#867,#538,#539,#540,#541),#683,.T.);
#5845=ADVANCED_FACE('',(#868),#5672,.T.);
#5846=ADVANCED_FACE('',(#869),#5673,.T.);
#5847=ADVANCED_FACE('',(#870,#542),#684,.T.);
#5848=ADVANCED_FACE('',(#871,#543,#544,#545),#685,.F.);
#5849=ADVANCED_FACE('',(#872),#686,.T.);
#5850=ADVANCED_FACE('',(#873),#5674,.F.);
#5851=ADVANCED_FACE('',(#874),#687,.T.);
#5852=ADVANCED_FACE('',(#875,#546),#5675,.F.);
#5853=ADVANCED_FACE('',(#876,#547),#5676,.T.);
#5854=ADVANCED_FACE('',(#877,#548),#688,.T.);
#5855=ADVANCED_FACE('',(#878,#549),#689,.F.);
#5856=ADVANCED_FACE('',(#879),#5677,.F.);
#5857=ADVANCED_FACE('',(#880),#690,.F.);
#5858=ADVANCED_FACE('',(#881),#5678,.F.);
#5859=ADVANCED_FACE('',(#882,#550,#551),#5679,.T.);
#5860=ADVANCED_FACE('',(#883),#691,.T.);
#5861=ADVANCED_FACE('',(#884,#552),#692,.F.);
#5862=ADVANCED_FACE('',(#885),#5680,.T.);
#5863=ADVANCED_FACE('',(#886),#693,.T.);
#5864=ADVANCED_FACE('',(#887),#694,.F.);
#5865=ADVANCED_FACE('',(#888),#695,.T.);
#5866=ADVANCED_FACE('',(#889),#5681,.T.);
#5867=ADVANCED_FACE('',(#890),#696,.F.);
#5868=ADVANCED_FACE('',(#891),#697,.T.);
#5869=ADVANCED_FACE('',(#892),#315,.T.);
#5870=ADVANCED_FACE('',(#893),#5682,.T.);
#5871=ADVANCED_FACE('',(#894),#698,.T.);
#5872=ADVANCED_FACE('',(#895),#699,.F.);
#5873=ADVANCED_FACE('',(#896),#700,.F.);
#5874=ADVANCED_FACE('',(#897),#5683,.F.);
#5875=ADVANCED_FACE('',(#898),#701,.F.);
#5876=ADVANCED_FACE('',(#899),#5684,.F.);
#5877=ADVANCED_FACE('',(#900,#553),#702,.T.);
#5878=ADVANCED_FACE('',(#901),#703,.T.);
#5879=ADVANCED_FACE('',(#902,#554),#704,.T.);
#5880=ADVANCED_FACE('',(#903),#705,.T.);
#5881=ADVANCED_FACE('',(#904),#706,.T.);
#5882=ADVANCED_FACE('',(#905,#555),#707,.F.);
#5883=ADVANCED_FACE('',(#906),#293,.F.);
#5884=ADVANCED_FACE('',(#907),#5685,.F.);
#5885=ADVANCED_FACE('',(#908,#556),#708,.T.);
#5886=ADVANCED_FACE('',(#909),#5686,.T.);
#5887=ADVANCED_FACE('',(#910,#557),#709,.F.);
#5888=ADVANCED_FACE('',(#911),#710,.T.);
#5889=ADVANCED_FACE('',(#912),#294,.T.);
#5890=ADVANCED_FACE('',(#913),#5687,.T.);
#5891=ADVANCED_FACE('',(#914),#295,.T.);
#5892=ADVANCED_FACE('',(#915,#558),#711,.T.);
#5893=ADVANCED_FACE('',(#916),#296,.T.);
#5894=ADVANCED_FACE('',(#917),#5688,.T.);
#5895=ADVANCED_FACE('',(#918),#297,.T.);
#5896=ADVANCED_FACE('',(#919),#712,.T.);
#5897=ADVANCED_FACE('',(#920),#713,.F.);
#5898=ADVANCED_FACE('',(#921),#714,.F.);
#5899=ADVANCED_FACE('',(#922),#715,.F.);
#5900=ADVANCED_FACE('',(#923),#716,.F.);
#5901=ADVANCED_FACE('',(#924),#717,.F.);
#5902=ADVANCED_FACE('',(#925),#718,.F.);
#5903=ADVANCED_FACE('',(#926),#719,.F.);
#5904=ADVANCED_FACE('',(#927),#720,.F.);
#5905=ADVANCED_FACE('',(#928),#298,.T.);
#5906=ADVANCED_FACE('',(#929),#299,.T.);
#5907=ADVANCED_FACE('',(#930),#721,.T.);
#5908=ADVANCED_FACE('',(#931),#722,.T.);
#5909=ADVANCED_FACE('',(#932),#723,.T.);
#5910=ADVANCED_FACE('',(#933),#5689,.F.);
#5911=ADVANCED_FACE('',(#934),#724,.T.);
#5912=ADVANCED_FACE('',(#935),#725,.T.);
#5913=ADVANCED_FACE('',(#936),#726,.T.);
#5914=ADVANCED_FACE('',(#937,#559),#727,.T.);
#5915=ADVANCED_FACE('',(#938,#560),#728,.F.);
#5916=ADVANCED_FACE('',(#939),#729,.T.);
#5917=ADVANCED_FACE('',(#940),#300,.T.);
#5918=ADVANCED_FACE('',(#941),#5690,.T.);
#5919=ADVANCED_FACE('',(#942),#301,.T.);
#5920=ADVANCED_FACE('',(#943,#561),#730,.T.);
#5921=ADVANCED_FACE('',(#944),#302,.T.);
#5922=ADVANCED_FACE('',(#945),#5691,.T.);
#5923=ADVANCED_FACE('',(#946),#303,.T.);
#5924=ADVANCED_FACE('',(#947),#731,.T.);
#5925=ADVANCED_FACE('',(#948),#732,.F.);
#5926=ADVANCED_FACE('',(#949),#733,.F.);
#5927=ADVANCED_FACE('',(#950),#734,.F.);
#5928=ADVANCED_FACE('',(#951),#735,.F.);
#5929=ADVANCED_FACE('',(#952),#736,.F.);
#5930=ADVANCED_FACE('',(#953),#737,.F.);
#5931=ADVANCED_FACE('',(#954),#738,.F.);
#5932=ADVANCED_FACE('',(#955),#739,.F.);
#5933=ADVANCED_FACE('',(#956),#5692,.F.);
#5934=ADVANCED_FACE('',(#957),#5693,.F.);
#5935=ADVANCED_FACE('',(#958),#5694,.F.);
#5936=ADVANCED_FACE('',(#959),#5695,.F.);
#5937=ADVANCED_FACE('',(#960),#5696,.F.);
#5938=ADVANCED_FACE('',(#961),#5697,.F.);
#5939=ADVANCED_FACE('',(#962),#5698,.F.);
#5940=ADVANCED_FACE('',(#963),#5699,.F.);
#5941=ADVANCED_FACE('',(#964),#5700,.F.);
#5942=ADVANCED_FACE('',(#965),#5701,.F.);
#5943=ADVANCED_FACE('',(#966),#5702,.T.);
#5944=ADVANCED_FACE('',(#967),#740,.T.);
#5945=ADVANCED_FACE('',(#968,#562,#563,#564,#565,#566,#567,#568,#569,#570,
#571),#741,.F.);
#5946=ADVANCED_FACE('',(#969),#742,.T.);
#5947=ADVANCED_FACE('',(#970),#5703,.T.);
#5948=ADVANCED_FACE('',(#971,#572,#573,#574,#575,#576,#577,#578,#579,#580,
#581),#743,.T.);
#5949=ADVANCED_FACE('',(#972),#5704,.F.);
#5950=ADVANCED_FACE('',(#973),#5705,.F.);
#5951=ADVANCED_FACE('',(#974),#5706,.F.);
#5952=ADVANCED_FACE('',(#975),#5707,.F.);
#5953=ADVANCED_FACE('',(#976),#5708,.T.);
#5954=ADVANCED_FACE('',(#977,#582),#744,.T.);
#5955=ADVANCED_FACE('',(#978),#5709,.F.);
#5956=ADVANCED_FACE('',(#979),#5710,.T.);
#5957=ADVANCED_FACE('',(#980,#583,#584,#585,#586,#587),#745,.T.);
#5958=ADVANCED_FACE('',(#981,#588,#589,#590,#591,#592),#746,.F.);
#5959=ADVANCED_FACE('',(#982),#5711,.F.);
#5960=ADVANCED_FACE('',(#983),#5712,.F.);
#5961=ADVANCED_FACE('',(#984),#5713,.F.);
#5962=ADVANCED_FACE('',(#985),#5714,.F.);
#5963=ADVANCED_FACE('',(#986),#5715,.T.);
#5964=ADVANCED_FACE('',(#987,#593),#747,.F.);
#5965=ADVANCED_FACE('',(#988),#5716,.F.);
#5966=ADVANCED_FACE('',(#989),#5717,.T.);
#5967=ADVANCED_FACE('',(#990,#594,#595,#596,#597,#598),#748,.T.);
#5968=ADVANCED_FACE('',(#991,#599,#600,#601,#602,#603),#749,.F.);
#5969=ADVANCED_FACE('',(#992),#5718,.F.);
#5970=ADVANCED_FACE('',(#993),#5719,.F.);
#5971=ADVANCED_FACE('',(#994),#5720,.F.);
#5972=ADVANCED_FACE('',(#995),#5721,.F.);
#5973=ADVANCED_FACE('',(#996),#5722,.T.);
#5974=ADVANCED_FACE('',(#997,#604),#750,.T.);
#5975=ADVANCED_FACE('',(#998),#5723,.F.);
#5976=ADVANCED_FACE('',(#999),#5724,.T.);
#5977=ADVANCED_FACE('',(#1000,#605,#606,#607,#608,#609),#751,.T.);
#5978=ADVANCED_FACE('',(#1001,#610,#611,#612,#613,#614),#752,.F.);
#5979=ADVANCED_FACE('',(#1002),#5725,.F.);
#5980=ADVANCED_FACE('',(#1003),#5726,.F.);
#5981=ADVANCED_FACE('',(#1004),#5727,.F.);
#5982=ADVANCED_FACE('',(#1005),#5728,.F.);
#5983=ADVANCED_FACE('',(#1006),#5729,.T.);
#5984=ADVANCED_FACE('',(#1007,#615),#753,.F.);
#5985=ADVANCED_FACE('',(#1008),#5730,.F.);
#5986=ADVANCED_FACE('',(#1009),#5731,.T.);
#5987=ADVANCED_FACE('',(#1010,#616,#617,#618,#619,#620),#754,.T.);
#5988=ADVANCED_FACE('',(#1011,#621,#622,#623,#624,#625),#755,.F.);
#5989=ADVANCED_FACE('',(#1012),#5732,.F.);
#5990=ADVANCED_FACE('',(#1013,#626),#5733,.T.);
#5991=ADVANCED_FACE('',(#1014),#756,.T.);
#5992=ADVANCED_FACE('',(#1015),#757,.T.);
#5993=ADVANCED_FACE('',(#1016),#758,.T.);
#5994=ADVANCED_FACE('',(#1017),#759,.T.);
#5995=ADVANCED_FACE('',(#1018),#760,.T.);
#5996=ADVANCED_FACE('',(#1019),#761,.T.);
#5997=ADVANCED_FACE('',(#1020),#762,.T.);
#5998=ADVANCED_FACE('',(#1021),#763,.T.);
#5999=ADVANCED_FACE('',(#1022),#764,.F.);
#6000=ADVANCED_FACE('',(#1023),#271,.F.);
#6001=ADVANCED_FACE('',(#1024),#5734,.T.);
#6002=ADVANCED_FACE('',(#1025),#5735,.F.);
#6003=ADVANCED_FACE('',(#1026),#304,.F.);
#6004=ADVANCED_FACE('',(#1027,#627),#765,.T.);
#6005=ADVANCED_FACE('',(#1028),#5736,.T.);
#6006=ADVANCED_FACE('',(#1029,#628),#766,.T.);
#6007=ADVANCED_FACE('',(#1030),#305,.F.);
#6008=ADVANCED_FACE('',(#1031),#272,.F.);
#6009=ADVANCED_FACE('',(#1032),#5737,.F.);
#6010=ADVANCED_FACE('',(#1033,#629),#767,.T.);
#6011=ADVANCED_FACE('',(#1034),#306,.T.);
#6012=ADVANCED_FACE('',(#1035),#5738,.T.);
#6013=ADVANCED_FACE('',(#1036),#307,.T.);
#6014=ADVANCED_FACE('',(#1037,#630),#768,.T.);
#6015=ADVANCED_FACE('',(#1038),#5739,.F.);
#6016=ADVANCED_FACE('',(#1039),#255,.T.);
#6017=ADVANCED_FACE('',(#1040),#256,.T.);
#6018=ADVANCED_FACE('',(#1041),#257,.T.);
#6019=ADVANCED_FACE('',(#1042),#258,.T.);
#6020=ADVANCED_FACE('',(#1043),#259,.T.);
#6021=ADVANCED_FACE('',(#1044),#260,.T.);
#6022=ADVANCED_FACE('',(#1045),#261,.T.);
#6023=ADVANCED_FACE('',(#1046),#262,.T.);
#6024=ADVANCED_FACE('',(#1047),#263,.F.);
#6025=ADVANCED_FACE('',(#1048),#5740,.T.);
#6026=ADVANCED_FACE('',(#1049),#769,.T.);
#6027=ADVANCED_FACE('',(#1050),#264,.F.);
#6028=ADVANCED_FACE('',(#1051),#770,.T.);
#6029=ADVANCED_FACE('',(#1052),#265,.F.);
#6030=ADVANCED_FACE('',(#1053),#771,.T.);
#6031=ADVANCED_FACE('',(#1054),#266,.F.);
#6032=ADVANCED_FACE('',(#1055),#772,.T.);
#6033=ADVANCED_FACE('',(#1056),#267,.F.);
#6034=ADVANCED_FACE('',(#1057),#773,.T.);
#6035=ADVANCED_FACE('',(#1058),#268,.F.);
#6036=ADVANCED_FACE('',(#1059),#774,.T.);
#6037=ADVANCED_FACE('',(#1060),#269,.F.);
#6038=ADVANCED_FACE('',(#1061),#5741,.F.);
#6039=ADVANCED_FACE('',(#1062),#775,.T.);
#6040=ADVANCED_FACE('',(#1063),#270,.F.);
#6041=ADVANCED_FACE('',(#1064,#631),#776,.T.);
#6042=ADVANCED_FACE('',(#1065),#777,.T.);
#6043=ADVANCED_FACE('',(#1066,#632),#778,.T.);
#6044=ADVANCED_FACE('',(#1067),#5742,.T.);
#6045=ADVANCED_FACE('',(#1068,#633),#779,.T.);
#6046=ADVANCED_FACE('',(#1069),#5743,.F.);
#6047=ADVANCED_FACE('',(#1070,#634),#780,.T.);
#6048=ADVANCED_FACE('',(#1071),#5744,.T.);
#6049=ADVANCED_FACE('',(#1072,#635),#781,.T.);
#6050=ADVANCED_FACE('',(#1073),#5745,.F.);
#6051=ADVANCED_FACE('',(#1074),#782,.F.);
#6052=ADVANCED_FACE('',(#1075),#783,.T.);
#6053=ADVANCED_FACE('',(#1076),#308,.T.);
#6054=ADVANCED_FACE('',(#1077),#5746,.T.);
#6055=ADVANCED_FACE('',(#1078),#309,.T.);
#6056=ADVANCED_FACE('',(#1079,#636),#784,.T.);
#6057=ADVANCED_FACE('',(#1080),#310,.T.);
#6058=ADVANCED_FACE('',(#1081),#5747,.T.);
#6059=ADVANCED_FACE('',(#1082),#785,.F.);
#6060=ADVANCED_FACE('',(#1083),#786,.F.);
#6061=ADVANCED_FACE('',(#1084),#787,.F.);
#6062=ADVANCED_FACE('',(#1085),#788,.F.);
#6063=ADVANCED_FACE('',(#1086),#789,.F.);
#6064=ADVANCED_FACE('',(#1087),#790,.F.);
#6065=ADVANCED_FACE('',(#1088),#791,.F.);
#6066=ADVANCED_FACE('',(#1089),#792,.F.);
#6067=ADVANCED_FACE('',(#1090),#5748,.F.);
#6068=ADVANCED_FACE('',(#1091),#793,.T.);
#6069=ADVANCED_FACE('',(#1092),#5749,.T.);
#6070=ADVANCED_FACE('',(#1093,#637),#794,.T.);
#6071=ADVANCED_FACE('',(#1094,#638),#795,.F.);
#6072=ADVANCED_FACE('',(#1095),#5750,.T.);
#6073=ADVANCED_FACE('',(#1096),#5751,.T.);
#6074=ADVANCED_FACE('',(#1097,#639),#796,.T.);
#6075=ADVANCED_FACE('',(#1098),#797,.F.);
#6076=ADVANCED_FACE('',(#1099),#798,.T.);
#6077=ADVANCED_FACE('',(#1100),#5752,.F.);
#6078=ADVANCED_FACE('',(#1101),#799,.T.);
#6079=ADVANCED_FACE('',(#1102,#640),#5753,.F.);
#6080=ADVANCED_FACE('',(#1103,#641),#5754,.T.);
#6081=ADVANCED_FACE('',(#1104,#642),#800,.T.);
#6082=ADVANCED_FACE('',(#1105,#643),#801,.F.);
#6083=ADVANCED_FACE('',(#1106),#5755,.F.);
#6084=ADVANCED_FACE('',(#1107),#5756,.T.);
#6085=ADVANCED_FACE('',(#1108,#644),#802,.T.);
#6086=ADVANCED_FACE('',(#1109,#645),#803,.F.);
#6087=ADVANCED_FACE('',(#1110),#5757,.F.);
#6088=ADVANCED_FACE('',(#1111),#5758,.T.);
#6089=ADVANCED_FACE('',(#1112,#646),#804,.T.);
#6090=ADVANCED_FACE('',(#1113,#647),#805,.F.);
#6091=ADVANCED_FACE('',(#1114),#5759,.T.);
#6092=ADVANCED_FACE('',(#1115),#806,.T.);
#6093=ADVANCED_FACE('',(#1116),#807,.F.);
#6094=ADVANCED_FACE('',(#1117),#5760,.T.);
#6095=ADVANCED_FACE('',(#1118),#808,.T.);
#6096=ADVANCED_FACE('',(#1119),#809,.F.);
#6097=ADVANCED_FACE('',(#1120),#5761,.F.);
#6098=ADVANCED_FACE('',(#1121),#5762,.T.);
#6099=ADVANCED_FACE('',(#1122,#648),#810,.T.);
#6100=ADVANCED_FACE('',(#1123,#649),#811,.F.);
#6101=ADVANCED_FACE('',(#1124),#812,.F.);
#6102=ADVANCED_FACE('',(#1125),#813,.F.);
#6103=ADVANCED_FACE('',(#1126),#814,.F.);
#6104=ADVANCED_FACE('',(#1127),#815,.F.);
#6105=ADVANCED_FACE('',(#1128),#816,.F.);
#6106=ADVANCED_FACE('',(#1129),#817,.F.);
#6107=ADVANCED_FACE('',(#1130),#818,.F.);
#6108=ADVANCED_FACE('',(#1131),#819,.F.);
#6109=ADVANCED_FACE('',(#1132,#650),#820,.T.);
#6110=ADVANCED_FACE('',(#1133),#311,.T.);
#6111=ADVANCED_FACE('',(#1134),#5763,.T.);
#6112=ADVANCED_FACE('',(#1135),#5764,.F.);
#6113=ADVANCED_FACE('',(#1136),#5765,.F.);
#6114=ADVANCED_FACE('',(#1137,#651,#652,#653),#5766,.T.);
#6115=ADVANCED_FACE('',(#1138),#5767,.F.);
#6116=ADVANCED_FACE('',(#1139),#5768,.F.);
#6117=ADVANCED_FACE('',(#1140,#654,#655,#656),#5769,.F.);
#6118=ADVANCED_FACE('',(#1141,#657),#821,.F.);
#6119=ADVANCED_FACE('',(#1142,#658),#822,.T.);
#6120=ADVANCED_FACE('',(#1143),#5770,.T.);
#6121=ADVANCED_FACE('',(#1144,#659),#823,.F.);
#6122=ADVANCED_FACE('',(#1145,#660),#824,.F.);
#6123=ADVANCED_FACE('',(#1146),#5771,.T.);
#6124=ADVANCED_FACE('',(#1147,#661),#825,.T.);
#6125=ADVANCED_FACE('',(#1148),#5772,.F.);
#6126=ADVANCED_FACE('',(#1149),#5773,.T.);
#6127=ADVANCED_FACE('',(#1150),#5774,.F.);
#6128=ADVANCED_FACE('',(#1151),#5775,.T.);
#6129=ADVANCED_FACE('',(#1152),#5776,.F.);
#6130=ADVANCED_FACE('',(#1153),#5777,.T.);
#6131=ADVANCED_FACE('',(#1154),#5778,.F.);
#6132=ADVANCED_FACE('',(#1155),#5779,.T.);
#6133=ADVANCED_FACE('',(#1156),#5780,.F.);
#6134=ADVANCED_FACE('',(#1157),#5781,.T.);
#6135=ADVANCED_FACE('',(#1158),#5782,.F.);
#6136=ADVANCED_FACE('',(#1159),#5783,.T.);
#6137=ADVANCED_FACE('',(#1160),#5784,.F.);
#6138=ADVANCED_FACE('',(#1161),#5785,.T.);
#6139=ADVANCED_FACE('',(#1162),#5786,.F.);
#6140=ADVANCED_FACE('',(#1163),#5787,.T.);
#6141=ADVANCED_FACE('',(#1164),#5788,.F.);
#6142=ADVANCED_FACE('',(#1165),#5789,.T.);
#6143=ADVANCED_FACE('',(#1166),#5790,.F.);
#6144=ADVANCED_FACE('',(#1167),#5791,.T.);
#6145=ADVANCED_FACE('',(#1168),#5792,.F.);
#6146=ADVANCED_FACE('',(#1169),#5793,.T.);
#6147=ADVANCED_FACE('',(#1170),#5794,.F.);
#6148=ADVANCED_FACE('',(#1171),#5795,.T.);
#6149=ADVANCED_FACE('',(#1172),#5796,.F.);
#6150=ADVANCED_FACE('',(#1173),#5797,.T.);
#6151=ADVANCED_FACE('',(#1174),#5798,.F.);
#6152=ADVANCED_FACE('',(#1175),#5799,.T.);
#6153=ADVANCED_FACE('',(#1176),#5800,.F.);
#6154=ADVANCED_FACE('',(#1177),#5801,.T.);
#6155=ADVANCED_FACE('',(#1178),#5802,.F.);
#6156=ADVANCED_FACE('',(#1179),#5803,.T.);
#6157=ADVANCED_FACE('',(#1180),#5804,.F.);
#6158=ADVANCED_FACE('',(#1181),#5805,.T.);
#6159=ADVANCED_FACE('',(#1182),#5806,.F.);
#6160=ADVANCED_FACE('',(#1183),#5807,.T.);
#6161=ADVANCED_FACE('',(#1184),#5808,.F.);
#6162=ADVANCED_FACE('',(#1185),#5809,.T.);
#6163=ADVANCED_FACE('',(#1186),#5810,.F.);
#6164=ADVANCED_FACE('',(#1187),#5811,.T.);
#6165=ADVANCED_FACE('',(#1188),#826,.F.);
#6166=ADVANCED_FACE('',(#1189),#827,.F.);
#6167=ADVANCED_FACE('',(#1190),#828,.F.);
#6168=ADVANCED_FACE('',(#1191),#829,.F.);
#6169=ADVANCED_FACE('',(#1192),#830,.F.);
#6170=ADVANCED_FACE('',(#1193),#831,.F.);
#6171=ADVANCED_FACE('',(#1194),#832,.F.);
#6172=ADVANCED_FACE('',(#1195),#833,.F.);
#6173=ADVANCED_FACE('',(#1196),#834,.F.);
#6174=ADVANCED_FACE('',(#1197),#835,.T.);
#6175=ADVANCED_FACE('',(#1198),#312,.T.);
#6176=ADVANCED_FACE('',(#1199),#5812,.T.);
#6177=ADVANCED_FACE('',(#1200),#313,.T.);
#6178=ADVANCED_FACE('',(#1201,#662),#836,.T.);
#6179=ADVANCED_FACE('',(#1202),#314,.T.);
#6180=ADVANCED_FACE('',(#1203),#5813,.T.);
#6181=CLOSED_SHELL('',(#5814,#5815,#5816,#5817,#5818,#5819,#5820,#5821,
#5822,#5823,#5824));
#6182=CLOSED_SHELL('',(#5825,#5826,#5827,#5828,#5829,#5830));
#6183=CLOSED_SHELL('',(#5831,#5832,#5833,#5834,#5835,#5836));
#6184=CLOSED_SHELL('',(#5837,#5838,#5839,#5840,#5841,#5842,#5843,#5844,
#5845,#5846,#5847,#5848));
#6185=CLOSED_SHELL('',(#5849,#5850,#5851,#5852,#5853,#5854,#5855));
#6186=CLOSED_SHELL('',(#5856,#5857,#5858,#5859,#5860,#5861));
#6187=CLOSED_SHELL('',(#5862,#5863,#5864,#5865,#5866,#5867,#5868,#5869,
#5870,#5871,#5872,#5873));
#6188=CLOSED_SHELL('',(#5874,#5875,#5876,#5877,#5878,#5879,#5880,#5881,
#5882));
#6189=CLOSED_SHELL('',(#5883,#5884,#5885,#5886,#5887));
#6190=CLOSED_SHELL('',(#5888,#5889,#5890,#5891,#5892,#5893,#5894,#5895,
#5896));
#6191=CLOSED_SHELL('',(#5897,#5898,#5899,#5900,#5901,#5902,#5903,#5904));
#6192=CLOSED_SHELL('',(#5905,#5906,#5907,#5908,#5909,#5910,#5911,#5912,
#5913,#5914,#5915));
#6193=CLOSED_SHELL('',(#5916,#5917,#5918,#5919,#5920,#5921,#5922,#5923,
#5924));
#6194=CLOSED_SHELL('',(#5925,#5926,#5927,#5928,#5929,#5930,#5931,#5932));
#6195=CLOSED_SHELL('',(#5933,#5934,#5935,#5936,#5937,#5938,#5939,#5940,
#5941,#5942,#5943,#5944,#5945,#5946,#5947,#5948));
#6196=CLOSED_SHELL('',(#5949,#5950,#5951,#5952,#5953,#5954,#5955,#5956,
#5957,#5958));
#6197=CLOSED_SHELL('',(#5959,#5960,#5961,#5962,#5963,#5964,#5965,#5966,
#5967,#5968));
#6198=CLOSED_SHELL('',(#5969,#5970,#5971,#5972,#5973,#5974,#5975,#5976,
#5977,#5978));
#6199=CLOSED_SHELL('',(#5979,#5980,#5981,#5982,#5983,#5984,#5985,#5986,
#5987,#5988));
#6200=CLOSED_SHELL('',(#5989,#5990,#5991,#5992,#5993,#5994,#5995,#5996,
#5997,#5998,#5999));
#6201=CLOSED_SHELL('',(#6000,#6001,#6002,#6003,#6004,#6005,#6006,#6007));
#6202=CLOSED_SHELL('',(#6008,#6009,#6010,#6011,#6012,#6013,#6014,#6015));
#6203=CLOSED_SHELL('',(#6016));
#6204=CLOSED_SHELL('',(#6017));
#6205=CLOSED_SHELL('',(#6018));
#6206=CLOSED_SHELL('',(#6019));
#6207=CLOSED_SHELL('',(#6020));
#6208=CLOSED_SHELL('',(#6021));
#6209=CLOSED_SHELL('',(#6022));
#6210=CLOSED_SHELL('',(#6023));
#6211=CLOSED_SHELL('',(#6024,#6025,#6026,#6027,#6028,#6029,#6030,#6031,
#6032,#6033,#6034,#6035,#6036,#6037,#6038,#6039,#6040,#6041,#6042));
#6212=CLOSED_SHELL('',(#6043,#6044,#6045,#6046));
#6213=CLOSED_SHELL('',(#6047,#6048,#6049,#6050));
#6214=CLOSED_SHELL('',(#6051,#6052,#6053,#6054,#6055,#6056,#6057,#6058));
#6215=CLOSED_SHELL('',(#6059,#6060,#6061,#6062,#6063,#6064,#6065,#6066));
#6216=CLOSED_SHELL('',(#6067,#6068,#6069,#6070,#6071,#6072,#6073,#6074,
#6075));
#6217=CLOSED_SHELL('',(#6076,#6077,#6078,#6079,#6080,#6081,#6082));
#6218=CLOSED_SHELL('',(#6083,#6084,#6085,#6086));
#6219=CLOSED_SHELL('',(#6087,#6088,#6089,#6090));
#6220=CLOSED_SHELL('',(#6091,#6092,#6093));
#6221=CLOSED_SHELL('',(#6094,#6095,#6096));
#6222=CLOSED_SHELL('',(#6097,#6098,#6099,#6100));
#6223=CLOSED_SHELL('',(#6101,#6102,#6103,#6104,#6105,#6106,#6107,#6108,
#6109,#6110,#6111));
#6224=CLOSED_SHELL('',(#6112,#6113,#6114,#6115,#6116,#6117,#6118,#6119,
#6120,#6121,#6122,#6123,#6124,#6125,#6126,#6127,#6128,#6129,#6130,#6131,
#6132,#6133,#6134,#6135,#6136,#6137,#6138,#6139,#6140,#6141,#6142,#6143,
#6144,#6145,#6146,#6147,#6148,#6149,#6150,#6151,#6152,#6153,#6154,#6155,
#6156,#6157,#6158,#6159,#6160,#6161,#6162,#6163,#6164));
#6225=CLOSED_SHELL('',(#6165,#6166,#6167,#6168,#6169,#6170,#6171,#6172));
#6226=CLOSED_SHELL('',(#6173,#6174,#6175,#6176,#6177,#6178,#6179,#6180));
#6227=DERIVED_UNIT_ELEMENT(#6295,1.);
#6228=DERIVED_UNIT_ELEMENT(#12781,-3.);
#6229=DERIVED_UNIT_ELEMENT(#6295,1.);
#6230=DERIVED_UNIT_ELEMENT(#12781,-3.);
#6231=DERIVED_UNIT_ELEMENT(#6295,1.);
#6232=DERIVED_UNIT_ELEMENT(#12781,-3.);
#6233=DERIVED_UNIT_ELEMENT(#6295,1.);
#6234=DERIVED_UNIT_ELEMENT(#12781,-3.);
#6235=DERIVED_UNIT_ELEMENT(#6295,1.);
#6236=DERIVED_UNIT_ELEMENT(#12781,-3.);
#6237=DERIVED_UNIT_ELEMENT(#6295,1.);
#6238=DERIVED_UNIT_ELEMENT(#12781,-3.);
#6239=DERIVED_UNIT_ELEMENT(#6295,1.);
#6240=DERIVED_UNIT_ELEMENT(#12781,-3.);
#6241=DERIVED_UNIT_ELEMENT(#6295,1.);
#6242=DERIVED_UNIT_ELEMENT(#12781,-3.);
#6243=DERIVED_UNIT_ELEMENT(#6295,1.);
#6244=DERIVED_UNIT_ELEMENT(#12781,-3.);
#6245=DERIVED_UNIT_ELEMENT(#6295,1.);
#6246=DERIVED_UNIT_ELEMENT(#12781,-3.);
#6247=DERIVED_UNIT_ELEMENT(#6295,1.);
#6248=DERIVED_UNIT_ELEMENT(#12781,-3.);
#6249=DERIVED_UNIT_ELEMENT(#6295,1.);
#6250=DERIVED_UNIT_ELEMENT(#12781,-3.);
#6251=DERIVED_UNIT_ELEMENT(#6295,1.);
#6252=DERIVED_UNIT_ELEMENT(#12781,-3.);
#6253=DERIVED_UNIT_ELEMENT(#6295,1.);
#6254=DERIVED_UNIT_ELEMENT(#12781,-3.);
#6255=DERIVED_UNIT_ELEMENT(#6295,1.);
#6256=DERIVED_UNIT_ELEMENT(#12781,-3.);
#6257=DERIVED_UNIT_ELEMENT(#6295,1.);
#6258=DERIVED_UNIT_ELEMENT(#12781,-3.);
#6259=DERIVED_UNIT_ELEMENT(#6295,1.);
#6260=DERIVED_UNIT_ELEMENT(#12781,-3.);
#6261=DERIVED_UNIT_ELEMENT(#6295,1.);
#6262=DERIVED_UNIT_ELEMENT(#12781,-3.);
#6263=DERIVED_UNIT_ELEMENT(#6295,1.);
#6264=DERIVED_UNIT_ELEMENT(#12781,-3.);
#6265=DERIVED_UNIT_ELEMENT(#6295,1.);
#6266=DERIVED_UNIT_ELEMENT(#12781,-3.);
#6267=DERIVED_UNIT_ELEMENT(#6295,1.);
#6268=DERIVED_UNIT_ELEMENT(#12781,-3.);
#6269=DERIVED_UNIT_ELEMENT(#6295,1.);
#6270=DERIVED_UNIT_ELEMENT(#12781,-3.);
#6271=DERIVED_UNIT_ELEMENT(#6295,1.);
#6272=DERIVED_UNIT_ELEMENT(#12781,-3.);
#6273=DERIVED_UNIT_ELEMENT(#6295,1.);
#6274=DERIVED_UNIT_ELEMENT(#12781,-3.);
#6275=DERIVED_UNIT_ELEMENT(#6295,1.);
#6276=DERIVED_UNIT_ELEMENT(#12781,-3.);
#6277=DERIVED_UNIT_ELEMENT(#6295,1.);
#6278=DERIVED_UNIT_ELEMENT(#12781,-3.);
#6279=DERIVED_UNIT_ELEMENT(#6295,1.);
#6280=DERIVED_UNIT_ELEMENT(#12781,-3.);
#6281=DERIVED_UNIT_ELEMENT(#6295,1.);
#6282=DERIVED_UNIT_ELEMENT(#12781,-3.);
#6283=DERIVED_UNIT_ELEMENT(#6295,1.);
#6284=DERIVED_UNIT_ELEMENT(#12781,-3.);
#6285=DERIVED_UNIT_ELEMENT(#6295,1.);
#6286=DERIVED_UNIT_ELEMENT(#12781,-3.);
#6287=DERIVED_UNIT_ELEMENT(#6295,1.);
#6288=DERIVED_UNIT_ELEMENT(#12781,-3.);
#6289=DERIVED_UNIT_ELEMENT(#6295,1.);
#6290=DERIVED_UNIT_ELEMENT(#12781,-3.);
#6291=DERIVED_UNIT_ELEMENT(#6295,1.);
#6292=DERIVED_UNIT_ELEMENT(#12781,-3.);
#6293=DERIVED_UNIT_ELEMENT(#6295,1.);
#6294=DERIVED_UNIT_ELEMENT(#12781,-3.);
#6295=(
MASS_UNIT()
NAMED_UNIT(*)
SI_UNIT(.KILO.,.GRAM.)
);
#6296=DERIVED_UNIT((#6227,#6228));
#6297=DERIVED_UNIT((#6229,#6230));
#6298=DERIVED_UNIT((#6231,#6232));
#6299=DERIVED_UNIT((#6233,#6234));
#6300=DERIVED_UNIT((#6235,#6236));
#6301=DERIVED_UNIT((#6237,#6238));
#6302=DERIVED_UNIT((#6239,#6240));
#6303=DERIVED_UNIT((#6241,#6242));
#6304=DERIVED_UNIT((#6243,#6244));
#6305=DERIVED_UNIT((#6245,#6246));
#6306=DERIVED_UNIT((#6247,#6248));
#6307=DERIVED_UNIT((#6249,#6250));
#6308=DERIVED_UNIT((#6251,#6252));
#6309=DERIVED_UNIT((#6253,#6254));
#6310=DERIVED_UNIT((#6255,#6256));
#6311=DERIVED_UNIT((#6257,#6258));
#6312=DERIVED_UNIT((#6259,#6260));
#6313=DERIVED_UNIT((#6261,#6262));
#6314=DERIVED_UNIT((#6263,#6264));
#6315=DERIVED_UNIT((#6265,#6266));
#6316=DERIVED_UNIT((#6267,#6268));
#6317=DERIVED_UNIT((#6269,#6270));
#6318=DERIVED_UNIT((#6271,#6272));
#6319=DERIVED_UNIT((#6273,#6274));
#6320=DERIVED_UNIT((#6275,#6276));
#6321=DERIVED_UNIT((#6277,#6278));
#6322=DERIVED_UNIT((#6279,#6280));
#6323=DERIVED_UNIT((#6281,#6282));
#6324=DERIVED_UNIT((#6283,#6284));
#6325=DERIVED_UNIT((#6285,#6286));
#6326=DERIVED_UNIT((#6287,#6288));
#6327=DERIVED_UNIT((#6289,#6290));
#6328=DERIVED_UNIT((#6291,#6292));
#6329=DERIVED_UNIT((#6293,#6294));
#6330=MEASURE_REPRESENTATION_ITEM('density measure',
POSITIVE_RATIO_MEASURE(7850.),#6296);
#6331=MEASURE_REPRESENTATION_ITEM('density measure',
POSITIVE_RATIO_MEASURE(7850.),#6297);
#6332=MEASURE_REPRESENTATION_ITEM('density measure',
POSITIVE_RATIO_MEASURE(7850.),#6298);
#6333=MEASURE_REPRESENTATION_ITEM('density measure',
POSITIVE_RATIO_MEASURE(7850.),#6299);
#6334=MEASURE_REPRESENTATION_ITEM('density measure',
POSITIVE_RATIO_MEASURE(7850.),#6300);
#6335=MEASURE_REPRESENTATION_ITEM('density measure',
POSITIVE_RATIO_MEASURE(7850.),#6301);
#6336=MEASURE_REPRESENTATION_ITEM('density measure',
POSITIVE_RATIO_MEASURE(7850.),#6302);
#6337=MEASURE_REPRESENTATION_ITEM('density measure',
POSITIVE_RATIO_MEASURE(7850.),#6303);
#6338=MEASURE_REPRESENTATION_ITEM('density measure',
POSITIVE_RATIO_MEASURE(7850.),#6304);
#6339=MEASURE_REPRESENTATION_ITEM('density measure',
POSITIVE_RATIO_MEASURE(7850.),#6305);
#6340=MEASURE_REPRESENTATION_ITEM('density measure',
POSITIVE_RATIO_MEASURE(7850.),#6306);
#6341=MEASURE_REPRESENTATION_ITEM('density measure',
POSITIVE_RATIO_MEASURE(7850.),#6307);
#6342=MEASURE_REPRESENTATION_ITEM('density measure',
POSITIVE_RATIO_MEASURE(7850.),#6308);
#6343=MEASURE_REPRESENTATION_ITEM('density measure',
POSITIVE_RATIO_MEASURE(7850.),#6309);
#6344=MEASURE_REPRESENTATION_ITEM('density measure',
POSITIVE_RATIO_MEASURE(7850.),#6310);
#6345=MEASURE_REPRESENTATION_ITEM('density measure',
POSITIVE_RATIO_MEASURE(7850.),#6311);
#6346=MEASURE_REPRESENTATION_ITEM('density measure',
POSITIVE_RATIO_MEASURE(7850.),#6312);
#6347=MEASURE_REPRESENTATION_ITEM('density measure',
POSITIVE_RATIO_MEASURE(7850.),#6313);
#6348=MEASURE_REPRESENTATION_ITEM('density measure',
POSITIVE_RATIO_MEASURE(7850.),#6314);
#6349=MEASURE_REPRESENTATION_ITEM('density measure',
POSITIVE_RATIO_MEASURE(7850.),#6315);
#6350=MEASURE_REPRESENTATION_ITEM('density measure',
POSITIVE_RATIO_MEASURE(7850.),#6316);
#6351=MEASURE_REPRESENTATION_ITEM('density measure',
POSITIVE_RATIO_MEASURE(7850.),#6317);
#6352=MEASURE_REPRESENTATION_ITEM('density measure',
POSITIVE_RATIO_MEASURE(7850.),#6318);
#6353=MEASURE_REPRESENTATION_ITEM('density measure',
POSITIVE_RATIO_MEASURE(7850.),#6319);
#6354=MEASURE_REPRESENTATION_ITEM('density measure',
POSITIVE_RATIO_MEASURE(7850.),#6320);
#6355=MEASURE_REPRESENTATION_ITEM('density measure',
POSITIVE_RATIO_MEASURE(7850.),#6321);
#6356=MEASURE_REPRESENTATION_ITEM('density measure',
POSITIVE_RATIO_MEASURE(7850.),#6322);
#6357=MEASURE_REPRESENTATION_ITEM('density measure',
POSITIVE_RATIO_MEASURE(7850.),#6323);
#6358=MEASURE_REPRESENTATION_ITEM('density measure',
POSITIVE_RATIO_MEASURE(7850.),#6324);
#6359=MEASURE_REPRESENTATION_ITEM('density measure',
POSITIVE_RATIO_MEASURE(7850.),#6325);
#6360=MEASURE_REPRESENTATION_ITEM('density measure',
POSITIVE_RATIO_MEASURE(7850.),#6326);
#6361=MEASURE_REPRESENTATION_ITEM('density measure',
POSITIVE_RATIO_MEASURE(7850.),#6327);
#6362=MEASURE_REPRESENTATION_ITEM('density measure',
POSITIVE_RATIO_MEASURE(7850.),#6328);
#6363=MEASURE_REPRESENTATION_ITEM('density measure',
POSITIVE_RATIO_MEASURE(7850.),#6329);
#6364=PROPERTY_DEFINITION_REPRESENTATION(#6534,#6432);
#6365=PROPERTY_DEFINITION_REPRESENTATION(#6535,#6433);
#6366=PROPERTY_DEFINITION_REPRESENTATION(#6536,#6434);
#6367=PROPERTY_DEFINITION_REPRESENTATION(#6537,#6435);
#6368=PROPERTY_DEFINITION_REPRESENTATION(#6538,#6436);
#6369=PROPERTY_DEFINITION_REPRESENTATION(#6539,#6437);
#6370=PROPERTY_DEFINITION_REPRESENTATION(#6540,#6438);
#6371=PROPERTY_DEFINITION_REPRESENTATION(#6541,#6439);
#6372=PROPERTY_DEFINITION_REPRESENTATION(#6542,#6440);
#6373=PROPERTY_DEFINITION_REPRESENTATION(#6543,#6441);
#6374=PROPERTY_DEFINITION_REPRESENTATION(#6544,#6442);
#6375=PROPERTY_DEFINITION_REPRESENTATION(#6545,#6443);
#6376=PROPERTY_DEFINITION_REPRESENTATION(#6546,#6444);
#6377=PROPERTY_DEFINITION_REPRESENTATION(#6547,#6445);
#6378=PROPERTY_DEFINITION_REPRESENTATION(#6548,#6446);
#6379=PROPERTY_DEFINITION_REPRESENTATION(#6549,#6447);
#6380=PROPERTY_DEFINITION_REPRESENTATION(#6550,#6448);
#6381=PROPERTY_DEFINITION_REPRESENTATION(#6551,#6449);
#6382=PROPERTY_DEFINITION_REPRESENTATION(#6552,#6450);
#6383=PROPERTY_DEFINITION_REPRESENTATION(#6553,#6451);
#6384=PROPERTY_DEFINITION_REPRESENTATION(#6554,#6452);
#6385=PROPERTY_DEFINITION_REPRESENTATION(#6555,#6453);
#6386=PROPERTY_DEFINITION_REPRESENTATION(#6556,#6454);
#6387=PROPERTY_DEFINITION_REPRESENTATION(#6557,#6455);
#6388=PROPERTY_DEFINITION_REPRESENTATION(#6558,#6456);
#6389=PROPERTY_DEFINITION_REPRESENTATION(#6559,#6457);
#6390=PROPERTY_DEFINITION_REPRESENTATION(#6560,#6458);
#6391=PROPERTY_DEFINITION_REPRESENTATION(#6561,#6459);
#6392=PROPERTY_DEFINITION_REPRESENTATION(#6562,#6460);
#6393=PROPERTY_DEFINITION_REPRESENTATION(#6563,#6461);
#6394=PROPERTY_DEFINITION_REPRESENTATION(#6564,#6462);
#6395=PROPERTY_DEFINITION_REPRESENTATION(#6565,#6463);
#6396=PROPERTY_DEFINITION_REPRESENTATION(#6566,#6464);
#6397=PROPERTY_DEFINITION_REPRESENTATION(#6567,#6465);
#6398=PROPERTY_DEFINITION_REPRESENTATION(#6568,#6466);
#6399=PROPERTY_DEFINITION_REPRESENTATION(#6569,#6467);
#6400=PROPERTY_DEFINITION_REPRESENTATION(#6570,#6468);
#6401=PROPERTY_DEFINITION_REPRESENTATION(#6571,#6469);
#6402=PROPERTY_DEFINITION_REPRESENTATION(#6572,#6470);
#6403=PROPERTY_DEFINITION_REPRESENTATION(#6573,#6471);
#6404=PROPERTY_DEFINITION_REPRESENTATION(#6574,#6472);
#6405=PROPERTY_DEFINITION_REPRESENTATION(#6575,#6473);
#6406=PROPERTY_DEFINITION_REPRESENTATION(#6576,#6474);
#6407=PROPERTY_DEFINITION_REPRESENTATION(#6577,#6475);
#6408=PROPERTY_DEFINITION_REPRESENTATION(#6578,#6476);
#6409=PROPERTY_DEFINITION_REPRESENTATION(#6579,#6477);
#6410=PROPERTY_DEFINITION_REPRESENTATION(#6580,#6478);
#6411=PROPERTY_DEFINITION_REPRESENTATION(#6581,#6479);
#6412=PROPERTY_DEFINITION_REPRESENTATION(#6582,#6480);
#6413=PROPERTY_DEFINITION_REPRESENTATION(#6583,#6481);
#6414=PROPERTY_DEFINITION_REPRESENTATION(#6584,#6482);
#6415=PROPERTY_DEFINITION_REPRESENTATION(#6585,#6483);
#6416=PROPERTY_DEFINITION_REPRESENTATION(#6586,#6484);
#6417=PROPERTY_DEFINITION_REPRESENTATION(#6587,#6485);
#6418=PROPERTY_DEFINITION_REPRESENTATION(#6588,#6486);
#6419=PROPERTY_DEFINITION_REPRESENTATION(#6589,#6487);
#6420=PROPERTY_DEFINITION_REPRESENTATION(#6590,#6488);
#6421=PROPERTY_DEFINITION_REPRESENTATION(#6591,#6489);
#6422=PROPERTY_DEFINITION_REPRESENTATION(#6592,#6490);
#6423=PROPERTY_DEFINITION_REPRESENTATION(#6593,#6491);
#6424=PROPERTY_DEFINITION_REPRESENTATION(#6594,#6492);
#6425=PROPERTY_DEFINITION_REPRESENTATION(#6595,#6493);
#6426=PROPERTY_DEFINITION_REPRESENTATION(#6596,#6494);
#6427=PROPERTY_DEFINITION_REPRESENTATION(#6597,#6495);
#6428=PROPERTY_DEFINITION_REPRESENTATION(#6598,#6496);
#6429=PROPERTY_DEFINITION_REPRESENTATION(#6599,#6497);
#6430=PROPERTY_DEFINITION_REPRESENTATION(#6600,#6498);
#6431=PROPERTY_DEFINITION_REPRESENTATION(#6601,#6499);
#6432=REPRESENTATION('material name',(#6500),#12742);
#6433=REPRESENTATION('density',(#6330),#12742);
#6434=REPRESENTATION('material name',(#6501),#12743);
#6435=REPRESENTATION('density',(#6331),#12743);
#6436=REPRESENTATION('material name',(#6502),#12744);
#6437=REPRESENTATION('density',(#6332),#12744);
#6438=REPRESENTATION('material name',(#6503),#12745);
#6439=REPRESENTATION('density',(#6333),#12745);
#6440=REPRESENTATION('material name',(#6504),#12746);
#6441=REPRESENTATION('density',(#6334),#12746);
#6442=REPRESENTATION('material name',(#6505),#12747);
#6443=REPRESENTATION('density',(#6335),#12747);
#6444=REPRESENTATION('material name',(#6506),#12748);
#6445=REPRESENTATION('density',(#6336),#12748);
#6446=REPRESENTATION('material name',(#6507),#12749);
#6447=REPRESENTATION('density',(#6337),#12749);
#6448=REPRESENTATION('material name',(#6508),#12750);
#6449=REPRESENTATION('density',(#6338),#12750);
#6450=REPRESENTATION('material name',(#6509),#12751);
#6451=REPRESENTATION('density',(#6339),#12751);
#6452=REPRESENTATION('material name',(#6510),#12752);
#6453=REPRESENTATION('density',(#6340),#12752);
#6454=REPRESENTATION('material name',(#6511),#12753);
#6455=REPRESENTATION('density',(#6341),#12753);
#6456=REPRESENTATION('material name',(#6512),#12755);
#6457=REPRESENTATION('density',(#6342),#12755);
#6458=REPRESENTATION('material name',(#6513),#12756);
#6459=REPRESENTATION('density',(#6343),#12756);
#6460=REPRESENTATION('material name',(#6514),#12757);
#6461=REPRESENTATION('density',(#6344),#12757);
#6462=REPRESENTATION('material name',(#6515),#12758);
#6463=REPRESENTATION('density',(#6345),#12758);
#6464=REPRESENTATION('material name',(#6516),#12759);
#6465=REPRESENTATION('density',(#6346),#12759);
#6466=REPRESENTATION('material name',(#6517),#12760);
#6467=REPRESENTATION('density',(#6347),#12760);
#6468=REPRESENTATION('material name',(#6518),#12762);
#6469=REPRESENTATION('density',(#6348),#12762);
#6470=REPRESENTATION('material name',(#6519),#12763);
#6471=REPRESENTATION('density',(#6349),#12763);
#6472=REPRESENTATION('material name',(#6520),#12764);
#6473=REPRESENTATION('density',(#6350),#12764);
#6474=REPRESENTATION('material name',(#6521),#12765);
#6475=REPRESENTATION('density',(#6351),#12765);
#6476=REPRESENTATION('material name',(#6522),#12766);
#6477=REPRESENTATION('density',(#6352),#12766);
#6478=REPRESENTATION('material name',(#6523),#12767);
#6479=REPRESENTATION('density',(#6353),#12767);
#6480=REPRESENTATION('material name',(#6524),#12769);
#6481=REPRESENTATION('density',(#6354),#12769);
#6482=REPRESENTATION('material name',(#6525),#12770);
#6483=REPRESENTATION('density',(#6355),#12770);
#6484=REPRESENTATION('material name',(#6526),#12771);
#6485=REPRESENTATION('density',(#6356),#12771);
#6486=REPRESENTATION('material name',(#6527),#12772);
#6487=REPRESENTATION('density',(#6357),#12772);
#6488=REPRESENTATION('material name',(#6528),#12773);
#6489=REPRESENTATION('density',(#6358),#12773);
#6490=REPRESENTATION('material name',(#6529),#12774);
#6491=REPRESENTATION('density',(#6359),#12774);
#6492=REPRESENTATION('material name',(#6530),#12775);
#6493=REPRESENTATION('density',(#6360),#12775);
#6494=REPRESENTATION('material name',(#6531),#12776);
#6495=REPRESENTATION('density',(#6361),#12776);
#6496=REPRESENTATION('material name',(#6532),#12777);
#6497=REPRESENTATION('density',(#6362),#12777);
#6498=REPRESENTATION('material name',(#6533),#12778);
#6499=REPRESENTATION('density',(#6363),#12778);
#6500=DESCRIPTIVE_REPRESENTATION_ITEM('Steel','Steel');
#6501=DESCRIPTIVE_REPRESENTATION_ITEM('Steel','Steel');
#6502=DESCRIPTIVE_REPRESENTATION_ITEM('Steel','Steel');
#6503=DESCRIPTIVE_REPRESENTATION_ITEM('Steel','Steel');
#6504=DESCRIPTIVE_REPRESENTATION_ITEM('Steel','Steel');
#6505=DESCRIPTIVE_REPRESENTATION_ITEM('Steel','Steel');
#6506=DESCRIPTIVE_REPRESENTATION_ITEM('Steel','Steel');
#6507=DESCRIPTIVE_REPRESENTATION_ITEM('Steel','Steel');
#6508=DESCRIPTIVE_REPRESENTATION_ITEM('Steel','Steel');
#6509=DESCRIPTIVE_REPRESENTATION_ITEM('Steel','Steel');
#6510=DESCRIPTIVE_REPRESENTATION_ITEM('Steel','Steel');
#6511=DESCRIPTIVE_REPRESENTATION_ITEM('Steel','Steel');
#6512=DESCRIPTIVE_REPRESENTATION_ITEM('Steel','Steel');
#6513=DESCRIPTIVE_REPRESENTATION_ITEM('Steel','Steel');
#6514=DESCRIPTIVE_REPRESENTATION_ITEM('Steel','Steel');
#6515=DESCRIPTIVE_REPRESENTATION_ITEM('Steel','Steel');
#6516=DESCRIPTIVE_REPRESENTATION_ITEM('Steel','Steel');
#6517=DESCRIPTIVE_REPRESENTATION_ITEM('Steel','Steel');
#6518=DESCRIPTIVE_REPRESENTATION_ITEM('Steel','Steel');
#6519=DESCRIPTIVE_REPRESENTATION_ITEM('Steel','Steel');
#6520=DESCRIPTIVE_REPRESENTATION_ITEM('Steel','Steel');
#6521=DESCRIPTIVE_REPRESENTATION_ITEM('Steel','Steel');
#6522=DESCRIPTIVE_REPRESENTATION_ITEM('Steel','Steel');
#6523=DESCRIPTIVE_REPRESENTATION_ITEM('Steel','Steel');
#6524=DESCRIPTIVE_REPRESENTATION_ITEM('Steel','Steel');
#6525=DESCRIPTIVE_REPRESENTATION_ITEM('Steel','Steel');
#6526=DESCRIPTIVE_REPRESENTATION_ITEM('Steel','Steel');
#6527=DESCRIPTIVE_REPRESENTATION_ITEM('Steel','Steel');
#6528=DESCRIPTIVE_REPRESENTATION_ITEM('Steel','Steel');
#6529=DESCRIPTIVE_REPRESENTATION_ITEM('Steel','Steel');
#6530=DESCRIPTIVE_REPRESENTATION_ITEM('Steel','Steel');
#6531=DESCRIPTIVE_REPRESENTATION_ITEM('Steel','Steel');
#6532=DESCRIPTIVE_REPRESENTATION_ITEM('Steel','Steel');
#6533=DESCRIPTIVE_REPRESENTATION_ITEM('Steel','Steel');
#6534=PROPERTY_DEFINITION('material property','material name',#12965);
#6535=PROPERTY_DEFINITION('material property','density of part',#12965);
#6536=PROPERTY_DEFINITION('material property','material name',#12966);
#6537=PROPERTY_DEFINITION('material property','density of part',#12966);
#6538=PROPERTY_DEFINITION('material property','material name',#12967);
#6539=PROPERTY_DEFINITION('material property','density of part',#12967);
#6540=PROPERTY_DEFINITION('material property','material name',#12968);
#6541=PROPERTY_DEFINITION('material property','density of part',#12968);
#6542=PROPERTY_DEFINITION('material property','material name',#12969);
#6543=PROPERTY_DEFINITION('material property','density of part',#12969);
#6544=PROPERTY_DEFINITION('material property','material name',#12970);
#6545=PROPERTY_DEFINITION('material property','density of part',#12970);
#6546=PROPERTY_DEFINITION('material property','material name',#12971);
#6547=PROPERTY_DEFINITION('material property','density of part',#12971);
#6548=PROPERTY_DEFINITION('material property','material name',#12972);
#6549=PROPERTY_DEFINITION('material property','density of part',#12972);
#6550=PROPERTY_DEFINITION('material property','material name',#12973);
#6551=PROPERTY_DEFINITION('material property','density of part',#12973);
#6552=PROPERTY_DEFINITION('material property','material name',#12974);
#6553=PROPERTY_DEFINITION('material property','density of part',#12974);
#6554=PROPERTY_DEFINITION('material property','material name',#12975);
#6555=PROPERTY_DEFINITION('material property','density of part',#12975);
#6556=PROPERTY_DEFINITION('material property','material name',#12976);
#6557=PROPERTY_DEFINITION('material property','density of part',#12976);
#6558=PROPERTY_DEFINITION('material property','material name',#12978);
#6559=PROPERTY_DEFINITION('material property','density of part',#12978);
#6560=PROPERTY_DEFINITION('material property','material name',#12979);
#6561=PROPERTY_DEFINITION('material property','density of part',#12979);
#6562=PROPERTY_DEFINITION('material property','material name',#12980);
#6563=PROPERTY_DEFINITION('material property','density of part',#12980);
#6564=PROPERTY_DEFINITION('material property','material name',#12981);
#6565=PROPERTY_DEFINITION('material property','density of part',#12981);
#6566=PROPERTY_DEFINITION('material property','material name',#12982);
#6567=PROPERTY_DEFINITION('material property','density of part',#12982);
#6568=PROPERTY_DEFINITION('material property','material name',#12983);
#6569=PROPERTY_DEFINITION('material property','density of part',#12983);
#6570=PROPERTY_DEFINITION('material property','material name',#12985);
#6571=PROPERTY_DEFINITION('material property','density of part',#12985);
#6572=PROPERTY_DEFINITION('material property','material name',#12986);
#6573=PROPERTY_DEFINITION('material property','density of part',#12986);
#6574=PROPERTY_DEFINITION('material property','material name',#12987);
#6575=PROPERTY_DEFINITION('material property','density of part',#12987);
#6576=PROPERTY_DEFINITION('material property','material name',#12988);
#6577=PROPERTY_DEFINITION('material property','density of part',#12988);
#6578=PROPERTY_DEFINITION('material property','material name',#12989);
#6579=PROPERTY_DEFINITION('material property','density of part',#12989);
#6580=PROPERTY_DEFINITION('material property','material name',#12990);
#6581=PROPERTY_DEFINITION('material property','density of part',#12990);
#6582=PROPERTY_DEFINITION('material property','material name',#12992);
#6583=PROPERTY_DEFINITION('material property','density of part',#12992);
#6584=PROPERTY_DEFINITION('material property','material name',#12993);
#6585=PROPERTY_DEFINITION('material property','density of part',#12993);
#6586=PROPERTY_DEFINITION('material property','material name',#12994);
#6587=PROPERTY_DEFINITION('material property','density of part',#12994);
#6588=PROPERTY_DEFINITION('material property','material name',#12995);
#6589=PROPERTY_DEFINITION('material property','density of part',#12995);
#6590=PROPERTY_DEFINITION('material property','material name',#12996);
#6591=PROPERTY_DEFINITION('material property','density of part',#12996);
#6592=PROPERTY_DEFINITION('material property','material name',#12997);
#6593=PROPERTY_DEFINITION('material property','density of part',#12997);
#6594=PROPERTY_DEFINITION('material property','material name',#12998);
#6595=PROPERTY_DEFINITION('material property','density of part',#12998);
#6596=PROPERTY_DEFINITION('material property','material name',#12999);
#6597=PROPERTY_DEFINITION('material property','density of part',#12999);
#6598=PROPERTY_DEFINITION('material property','material name',#13000);
#6599=PROPERTY_DEFINITION('material property','density of part',#13000);
#6600=PROPERTY_DEFINITION('material property','material name',#13001);
#6601=PROPERTY_DEFINITION('material property','density of part',#13001);
#6602=AXIS2_PLACEMENT_3D('',#9444,#7433,#7434);
#6603=AXIS2_PLACEMENT_3D('',#9445,#7435,#7436);
#6604=AXIS2_PLACEMENT_3D('',#9446,#7437,#7438);
#6605=AXIS2_PLACEMENT_3D('',#9447,#7439,#7440);
#6606=AXIS2_PLACEMENT_3D('',#9449,#7441,#7442);
#6607=AXIS2_PLACEMENT_3D('',#9452,#7444,#7445);
#6608=AXIS2_PLACEMENT_3D('',#9453,#7446,#7447);
#6609=AXIS2_PLACEMENT_3D('',#9455,#7448,#7449);
#6610=AXIS2_PLACEMENT_3D('',#9458,#7451,#7452);
#6611=AXIS2_PLACEMENT_3D('',#9459,#7453,#7454);
#6612=AXIS2_PLACEMENT_3D('',#9461,#7455,#7456);
#6613=AXIS2_PLACEMENT_3D('',#9464,#7458,#7459);
#6614=AXIS2_PLACEMENT_3D('',#9465,#7460,#7461);
#6615=AXIS2_PLACEMENT_3D('',#9467,#7462,#7463);
#6616=AXIS2_PLACEMENT_3D('',#9470,#7465,#7466);
#6617=AXIS2_PLACEMENT_3D('',#9471,#7467,#7468);
#6618=AXIS2_PLACEMENT_3D('',#9473,#7469,#7470);
#6619=AXIS2_PLACEMENT_3D('',#9476,#7472,#7473);
#6620=AXIS2_PLACEMENT_3D('',#9477,#7474,#7475);
#6621=AXIS2_PLACEMENT_3D('',#9486,#7480,#7481);
#6622=AXIS2_PLACEMENT_3D('',#9492,#7485,#7486);
#6623=AXIS2_PLACEMENT_3D('',#9498,#7490,#7491);
#6624=AXIS2_PLACEMENT_3D('',#9501,#7494,#7495);
#6625=AXIS2_PLACEMENT_3D('',#9502,#7496,#7497);
#6626=AXIS2_PLACEMENT_3D('',#9503,#7498,#7499);
#6627=AXIS2_PLACEMENT_3D('',#9504,#7500,#7501);
#6628=AXIS2_PLACEMENT_3D('',#9513,#7506,#7507);
#6629=AXIS2_PLACEMENT_3D('',#9519,#7511,#7512);
#6630=AXIS2_PLACEMENT_3D('',#9525,#7516,#7517);
#6631=AXIS2_PLACEMENT_3D('',#9528,#7520,#7521);
#6632=AXIS2_PLACEMENT_3D('',#9529,#7522,#7523);
#6633=AXIS2_PLACEMENT_3D('',#9530,#7524,#7525);
#6634=AXIS2_PLACEMENT_3D('',#9531,#7526,#7527);
#6635=AXIS2_PLACEMENT_3D('',#9540,#7532,#7533);
#6636=AXIS2_PLACEMENT_3D('',#9546,#7537,#7538);
#6637=AXIS2_PLACEMENT_3D('',#9552,#7542,#7543);
#6638=AXIS2_PLACEMENT_3D('',#9555,#7546,#7547);
#6639=AXIS2_PLACEMENT_3D('',#9556,#7548,#7549);
#6640=AXIS2_PLACEMENT_3D('',#9557,#7550,#7551);
#6641=AXIS2_PLACEMENT_3D('',#9558,#7552,#7553);
#6642=AXIS2_PLACEMENT_3D('',#9560,#7554,#7555);
#6643=AXIS2_PLACEMENT_3D('',#9563,#7557,#7558);
#6644=AXIS2_PLACEMENT_3D('',#9564,#7559,#7560);
#6645=AXIS2_PLACEMENT_3D('',#9566,#7561,#7562);
#6646=AXIS2_PLACEMENT_3D('',#9569,#7564,#7565);
#6647=AXIS2_PLACEMENT_3D('',#9570,#7566,#7567);
#6648=AXIS2_PLACEMENT_3D('',#9572,#7568,#7569);
#6649=AXIS2_PLACEMENT_3D('',#9575,#7571,#7572);
#6650=AXIS2_PLACEMENT_3D('',#9576,#7573,#7574);
#6651=AXIS2_PLACEMENT_3D('',#9578,#7575,#7576);
#6652=AXIS2_PLACEMENT_3D('',#9580,#7577,#7578);
#6653=AXIS2_PLACEMENT_3D('',#9581,#7579,#7580);
#6654=AXIS2_PLACEMENT_3D('',#9584,#7582,#7583);
#6655=AXIS2_PLACEMENT_3D('',#9585,#7584,#7585);
#6656=AXIS2_PLACEMENT_3D('',#9587,#7586,#7587);
#6657=AXIS2_PLACEMENT_3D('',#9589,#7589,#7590);
#6658=AXIS2_PLACEMENT_3D('',#9590,#7591,#7592);
#6659=AXIS2_PLACEMENT_3D('',#9592,#7593,#7594);
#6660=AXIS2_PLACEMENT_3D('',#9594,#7595,#7596);
#6661=AXIS2_PLACEMENT_3D('',#9595,#7597,#7598);
#6662=AXIS2_PLACEMENT_3D('',#9598,#7600,#7601);
#6663=AXIS2_PLACEMENT_3D('',#9599,#7602,#7603);
#6664=AXIS2_PLACEMENT_3D('',#9601,#7604,#7605);
#6665=AXIS2_PLACEMENT_3D('',#9603,#7607,#7608);
#6666=AXIS2_PLACEMENT_3D('',#9604,#7609,#7610);
#6667=AXIS2_PLACEMENT_3D('',#9605,#7611,#7612);
#6668=AXIS2_PLACEMENT_3D('',#9606,#7613,#7614);
#6669=AXIS2_PLACEMENT_3D('',#9610,#7616,#7617);
#6670=AXIS2_PLACEMENT_3D('',#9611,#7618,#7619);
#6671=AXIS2_PLACEMENT_3D('',#9628,#7620,#7621);
#6672=AXIS2_PLACEMENT_3D('',#9685,#7623,#7624);
#6673=AXIS2_PLACEMENT_3D('',#9687,#7626,#7627);
#6674=AXIS2_PLACEMENT_3D('',#9689,#7628,#7629);
#6675=AXIS2_PLACEMENT_3D('',#9692,#7631,#7632);
#6676=AXIS2_PLACEMENT_3D('',#9693,#7633,#7634);
#6677=AXIS2_PLACEMENT_3D('',#9695,#7635,#7636);
#6678=AXIS2_PLACEMENT_3D('',#9698,#7638,#7639);
#6679=AXIS2_PLACEMENT_3D('',#9699,#7640,#7641);
#6680=AXIS2_PLACEMENT_3D('',#9700,#7642,#7643);
#6681=AXIS2_PLACEMENT_3D('',#9701,#7644,#7645);
#6682=AXIS2_PLACEMENT_3D('',#9702,#7646,#7647);
#6683=AXIS2_PLACEMENT_3D('',#9704,#7648,#7649);
#6684=AXIS2_PLACEMENT_3D('',#9707,#7651,#7652);
#6685=AXIS2_PLACEMENT_3D('',#9708,#7653,#7654);
#6686=AXIS2_PLACEMENT_3D('',#9709,#7655,#7656);
#6687=AXIS2_PLACEMENT_3D('',#9781,#7658,#7659);
#6688=AXIS2_PLACEMENT_3D('',#9783,#7660,#7661);
#6689=AXIS2_PLACEMENT_3D('',#9786,#7663,#7664);
#6690=AXIS2_PLACEMENT_3D('',#9787,#7665,#7666);
#6691=AXIS2_PLACEMENT_3D('',#9788,#7667,#7668);
#6692=AXIS2_PLACEMENT_3D('',#9789,#7669,#7670);
#6693=AXIS2_PLACEMENT_3D('',#9790,#7671,#7672);
#6694=AXIS2_PLACEMENT_3D('',#9792,#7673,#7674);
#6695=AXIS2_PLACEMENT_3D('',#9796,#7676,#7677);
#6696=AXIS2_PLACEMENT_3D('',#9797,#7678,#7679);
#6697=AXIS2_PLACEMENT_3D('',#9798,#7680,#7681);
#6698=AXIS2_PLACEMENT_3D('',#9799,#7682,#7683);
#6699=AXIS2_PLACEMENT_3D('',#9801,#7685,#7686);
#6700=AXIS2_PLACEMENT_3D('',#9803,#7687,#7688);
#6701=AXIS2_PLACEMENT_3D('',#9804,#7689,#7690);
#6702=AXIS2_PLACEMENT_3D('',#9805,#7691,#7692);
#6703=AXIS2_PLACEMENT_3D('',#9808,#7693,#7694);
#6704=AXIS2_PLACEMENT_3D('',#9876,#7696,#7697);
#6705=AXIS2_PLACEMENT_3D('',#9878,#7699,#7700);
#6706=AXIS2_PLACEMENT_3D('',#9879,#7701,#7702);
#6707=AXIS2_PLACEMENT_3D('',#10354,#7703,#7704);
#6708=AXIS2_PLACEMENT_3D('',#10401,#7705,#7706);
#6709=AXIS2_PLACEMENT_3D('',#10402,#7707,#7708);
#6710=AXIS2_PLACEMENT_3D('',#10403,#7709,#7710);
#6711=AXIS2_PLACEMENT_3D('',#10406,#7712,#7713);
#6712=AXIS2_PLACEMENT_3D('',#10407,#7714,#7715);
#6713=AXIS2_PLACEMENT_3D('',#10409,#7717,#7718);
#6714=AXIS2_PLACEMENT_3D('',#10410,#7719,#7720);
#6715=AXIS2_PLACEMENT_3D('',#10411,#7721,#7722);
#6716=AXIS2_PLACEMENT_3D('',#10412,#7723,#7724);
#6717=AXIS2_PLACEMENT_3D('',#10414,#7725,#7726);
#6718=AXIS2_PLACEMENT_3D('',#10417,#7728,#7729);
#6719=AXIS2_PLACEMENT_3D('',#10418,#7730,#7731);
#6720=AXIS2_PLACEMENT_3D('',#10419,#7732,#7733);
#6721=AXIS2_PLACEMENT_3D('',#10421,#7734,#7735);
#6722=AXIS2_PLACEMENT_3D('',#10424,#7737,#7738);
#6723=AXIS2_PLACEMENT_3D('',#10425,#7739,#7740);
#6724=AXIS2_PLACEMENT_3D('',#10434,#7745,#7746);
#6725=AXIS2_PLACEMENT_3D('',#10440,#7750,#7751);
#6726=AXIS2_PLACEMENT_3D('',#10446,#7755,#7756);
#6727=AXIS2_PLACEMENT_3D('',#10449,#7759,#7760);
#6728=AXIS2_PLACEMENT_3D('',#10450,#7761,#7762);
#6729=AXIS2_PLACEMENT_3D('',#10451,#7763,#7764);
#6730=AXIS2_PLACEMENT_3D('',#10452,#7765,#7766);
#6731=AXIS2_PLACEMENT_3D('',#10454,#7767,#7768);
#6732=AXIS2_PLACEMENT_3D('',#10457,#7770,#7771);
#6733=AXIS2_PLACEMENT_3D('',#10458,#7772,#7773);
#6734=AXIS2_PLACEMENT_3D('',#10461,#7775,#7776);
#6735=AXIS2_PLACEMENT_3D('',#10462,#7777,#7778);
#6736=AXIS2_PLACEMENT_3D('',#10464,#7779,#7780);
#6737=AXIS2_PLACEMENT_3D('',#10465,#7781,#7782);
#6738=AXIS2_PLACEMENT_3D('',#10468,#7784,#7785);
#6739=AXIS2_PLACEMENT_3D('',#10469,#7786,#7787);
#6740=AXIS2_PLACEMENT_3D('',#10470,#7788,#7789);
#6741=AXIS2_PLACEMENT_3D('',#10471,#7790,#7791);
#6742=AXIS2_PLACEMENT_3D('',#10473,#7792,#7793);
#6743=AXIS2_PLACEMENT_3D('',#10474,#7794,#7795);
#6744=AXIS2_PLACEMENT_3D('',#10476,#7796,#7797);
#6745=AXIS2_PLACEMENT_3D('',#10478,#7799,#7800);
#6746=AXIS2_PLACEMENT_3D('',#10480,#7801,#7802);
#6747=AXIS2_PLACEMENT_3D('',#10482,#7804,#7805);
#6748=AXIS2_PLACEMENT_3D('',#10484,#7806,#7807);
#6749=AXIS2_PLACEMENT_3D('',#10486,#7809,#7810);
#6750=AXIS2_PLACEMENT_3D('',#10488,#7811,#7812);
#6751=AXIS2_PLACEMENT_3D('',#10489,#7813,#7814);
#6752=AXIS2_PLACEMENT_3D('',#10491,#7815,#7816);
#6753=AXIS2_PLACEMENT_3D('',#10493,#7818,#7819);
#6754=AXIS2_PLACEMENT_3D('',#10495,#7820,#7821);
#6755=AXIS2_PLACEMENT_3D('',#10497,#7823,#7824);
#6756=AXIS2_PLACEMENT_3D('',#10499,#7825,#7826);
#6757=AXIS2_PLACEMENT_3D('',#10501,#7828,#7829);
#6758=AXIS2_PLACEMENT_3D('',#10502,#7830,#7831);
#6759=AXIS2_PLACEMENT_3D('',#10511,#7836,#7837);
#6760=AXIS2_PLACEMENT_3D('',#10517,#7841,#7842);
#6761=AXIS2_PLACEMENT_3D('',#10523,#7846,#7847);
#6762=AXIS2_PLACEMENT_3D('',#10529,#7851,#7852);
#6763=AXIS2_PLACEMENT_3D('',#10535,#7856,#7857);
#6764=AXIS2_PLACEMENT_3D('',#10538,#7860,#7861);
#6765=AXIS2_PLACEMENT_3D('',#10539,#7862,#7863);
#6766=AXIS2_PLACEMENT_3D('',#10540,#7864,#7865);
#6767=AXIS2_PLACEMENT_3D('',#10541,#7866,#7867);
#6768=AXIS2_PLACEMENT_3D('',#10553,#7869,#7870);
#6769=AXIS2_PLACEMENT_3D('',#10569,#7871,#7872);
#6770=AXIS2_PLACEMENT_3D('',#10571,#7873,#7874);
#6771=AXIS2_PLACEMENT_3D('',#10597,#7876,#7877);
#6772=AXIS2_PLACEMENT_3D('',#10600,#7880,#7881);
#6773=AXIS2_PLACEMENT_3D('',#10602,#7883,#7884);
#6774=AXIS2_PLACEMENT_3D('',#10604,#7886,#7887);
#6775=AXIS2_PLACEMENT_3D('',#10606,#7888,#7889);
#6776=AXIS2_PLACEMENT_3D('',#10609,#7891,#7892);
#6777=AXIS2_PLACEMENT_3D('',#10610,#7893,#7894);
#6778=AXIS2_PLACEMENT_3D('',#10612,#7896,#7897);
#6779=AXIS2_PLACEMENT_3D('',#10614,#7899,#7900);
#6780=AXIS2_PLACEMENT_3D('',#10615,#7901,#7902);
#6781=AXIS2_PLACEMENT_3D('',#10616,#7903,#7904);
#6782=AXIS2_PLACEMENT_3D('',#10617,#7905,#7906);
#6783=AXIS2_PLACEMENT_3D('',#10618,#7907,#7908);
#6784=AXIS2_PLACEMENT_3D('',#10620,#7909,#7910);
#6785=AXIS2_PLACEMENT_3D('',#10621,#7911,#7912);
#6786=AXIS2_PLACEMENT_3D('',#10623,#7913,#7914);
#6787=AXIS2_PLACEMENT_3D('',#10625,#7916,#7917);
#6788=AXIS2_PLACEMENT_3D('',#10627,#7918,#7919);
#6789=AXIS2_PLACEMENT_3D('',#10629,#7921,#7922);
#6790=AXIS2_PLACEMENT_3D('',#10631,#7923,#7924);
#6791=AXIS2_PLACEMENT_3D('',#10633,#7926,#7927);
#6792=AXIS2_PLACEMENT_3D('',#10635,#7928,#7929);
#6793=AXIS2_PLACEMENT_3D('',#10636,#7930,#7931);
#6794=AXIS2_PLACEMENT_3D('',#10638,#7932,#7933);
#6795=AXIS2_PLACEMENT_3D('',#10640,#7935,#7936);
#6796=AXIS2_PLACEMENT_3D('',#10642,#7937,#7938);
#6797=AXIS2_PLACEMENT_3D('',#10644,#7940,#7941);
#6798=AXIS2_PLACEMENT_3D('',#10646,#7942,#7943);
#6799=AXIS2_PLACEMENT_3D('',#10648,#7945,#7946);
#6800=AXIS2_PLACEMENT_3D('',#10649,#7947,#7948);
#6801=AXIS2_PLACEMENT_3D('',#10658,#7953,#7954);
#6802=AXIS2_PLACEMENT_3D('',#10664,#7958,#7959);
#6803=AXIS2_PLACEMENT_3D('',#10670,#7963,#7964);
#6804=AXIS2_PLACEMENT_3D('',#10676,#7968,#7969);
#6805=AXIS2_PLACEMENT_3D('',#10682,#7973,#7974);
#6806=AXIS2_PLACEMENT_3D('',#10685,#7977,#7978);
#6807=AXIS2_PLACEMENT_3D('',#10686,#7979,#7980);
#6808=AXIS2_PLACEMENT_3D('',#10687,#7981,#7982);
#6809=AXIS2_PLACEMENT_3D('',#10688,#7983,#7984);
#6810=AXIS2_PLACEMENT_3D('',#10689,#7985,#7986);
#6811=AXIS2_PLACEMENT_3D('',#10691,#7987,#7988);
#6812=AXIS2_PLACEMENT_3D('',#10694,#7990,#7991);
#6813=AXIS2_PLACEMENT_3D('',#10695,#7992,#7993);
#6814=AXIS2_PLACEMENT_3D('',#10697,#7994,#7995);
#6815=AXIS2_PLACEMENT_3D('',#10700,#7997,#7998);
#6816=AXIS2_PLACEMENT_3D('',#10701,#7999,#8000);
#6817=AXIS2_PLACEMENT_3D('',#10703,#8001,#8002);
#6818=AXIS2_PLACEMENT_3D('',#10706,#8004,#8005);
#6819=AXIS2_PLACEMENT_3D('',#10707,#8006,#8007);
#6820=AXIS2_PLACEMENT_3D('',#10709,#8008,#8009);
#6821=AXIS2_PLACEMENT_3D('',#10712,#8011,#8012);
#6822=AXIS2_PLACEMENT_3D('',#10713,#8013,#8014);
#6823=AXIS2_PLACEMENT_3D('',#10715,#8015,#8016);
#6824=AXIS2_PLACEMENT_3D('',#10718,#8018,#8019);
#6825=AXIS2_PLACEMENT_3D('',#10719,#8020,#8021);
#6826=AXIS2_PLACEMENT_3D('',#10721,#8022,#8023);
#6827=AXIS2_PLACEMENT_3D('',#10724,#8025,#8026);
#6828=AXIS2_PLACEMENT_3D('',#10725,#8027,#8028);
#6829=AXIS2_PLACEMENT_3D('',#10727,#8029,#8030);
#6830=AXIS2_PLACEMENT_3D('',#10730,#8032,#8033);
#6831=AXIS2_PLACEMENT_3D('',#10731,#8034,#8035);
#6832=AXIS2_PLACEMENT_3D('',#10733,#8036,#8037);
#6833=AXIS2_PLACEMENT_3D('',#10736,#8039,#8040);
#6834=AXIS2_PLACEMENT_3D('',#10737,#8041,#8042);
#6835=AXIS2_PLACEMENT_3D('',#10739,#8043,#8044);
#6836=AXIS2_PLACEMENT_3D('',#10742,#8046,#8047);
#6837=AXIS2_PLACEMENT_3D('',#10743,#8048,#8049);
#6838=AXIS2_PLACEMENT_3D('',#10745,#8050,#8051);
#6839=AXIS2_PLACEMENT_3D('',#10748,#8053,#8054);
#6840=AXIS2_PLACEMENT_3D('',#10749,#8055,#8056);
#6841=AXIS2_PLACEMENT_3D('',#10754,#8058,#8059);
#6842=AXIS2_PLACEMENT_3D('',#10757,#8061,#8062);
#6843=AXIS2_PLACEMENT_3D('',#10758,#8063,#8064);
#6844=AXIS2_PLACEMENT_3D('',#10764,#8068,#8069);
#6845=AXIS2_PLACEMENT_3D('',#10767,#8071,#8072);
#6846=AXIS2_PLACEMENT_3D('',#10768,#8073,#8074);
#6847=AXIS2_PLACEMENT_3D('',#10772,#8077,#8078);
#6848=AXIS2_PLACEMENT_3D('',#10773,#8079,#8080);
#6849=AXIS2_PLACEMENT_3D('',#10774,#8081,#8082);
#6850=AXIS2_PLACEMENT_3D('',#10775,#8083,#8084);
#6851=AXIS2_PLACEMENT_3D('',#10776,#8085,#8086);
#6852=AXIS2_PLACEMENT_3D('',#10778,#8087,#8088);
#6853=AXIS2_PLACEMENT_3D('',#10781,#8090,#8091);
#6854=AXIS2_PLACEMENT_3D('',#10782,#8092,#8093);
#6855=AXIS2_PLACEMENT_3D('',#10784,#8094,#8095);
#6856=AXIS2_PLACEMENT_3D('',#10787,#8097,#8098);
#6857=AXIS2_PLACEMENT_3D('',#10788,#8099,#8100);
#6858=AXIS2_PLACEMENT_3D('',#10790,#8101,#8102);
#6859=AXIS2_PLACEMENT_3D('',#10793,#8104,#8105);
#6860=AXIS2_PLACEMENT_3D('',#10794,#8106,#8107);
#6861=AXIS2_PLACEMENT_3D('',#10796,#8108,#8109);
#6862=AXIS2_PLACEMENT_3D('',#10799,#8111,#8112);
#6863=AXIS2_PLACEMENT_3D('',#10800,#8113,#8114);
#6864=AXIS2_PLACEMENT_3D('',#10802,#8115,#8116);
#6865=AXIS2_PLACEMENT_3D('',#10805,#8118,#8119);
#6866=AXIS2_PLACEMENT_3D('',#10806,#8120,#8121);
#6867=AXIS2_PLACEMENT_3D('',#10808,#8122,#8123);
#6868=AXIS2_PLACEMENT_3D('',#10809,#8124,#8125);
#6869=AXIS2_PLACEMENT_3D('',#10812,#8127,#8128);
#6870=AXIS2_PLACEMENT_3D('',#10813,#8129,#8130);
#6871=AXIS2_PLACEMENT_3D('',#10815,#8131,#8132);
#6872=AXIS2_PLACEMENT_3D('',#10818,#8134,#8135);
#6873=AXIS2_PLACEMENT_3D('',#10819,#8136,#8137);
#6874=AXIS2_PLACEMENT_3D('',#10820,#8138,#8139);
#6875=AXIS2_PLACEMENT_3D('',#10821,#8140,#8141);
#6876=AXIS2_PLACEMENT_3D('',#10822,#8142,#8143);
#6877=AXIS2_PLACEMENT_3D('',#10824,#8144,#8145);
#6878=AXIS2_PLACEMENT_3D('',#10827,#8147,#8148);
#6879=AXIS2_PLACEMENT_3D('',#10828,#8149,#8150);
#6880=AXIS2_PLACEMENT_3D('',#10830,#8151,#8152);
#6881=AXIS2_PLACEMENT_3D('',#10833,#8154,#8155);
#6882=AXIS2_PLACEMENT_3D('',#10834,#8156,#8157);
#6883=AXIS2_PLACEMENT_3D('',#10836,#8158,#8159);
#6884=AXIS2_PLACEMENT_3D('',#10839,#8161,#8162);
#6885=AXIS2_PLACEMENT_3D('',#10840,#8163,#8164);
#6886=AXIS2_PLACEMENT_3D('',#10842,#8165,#8166);
#6887=AXIS2_PLACEMENT_3D('',#10845,#8168,#8169);
#6888=AXIS2_PLACEMENT_3D('',#10846,#8170,#8171);
#6889=AXIS2_PLACEMENT_3D('',#10848,#8172,#8173);
#6890=AXIS2_PLACEMENT_3D('',#10851,#8175,#8176);
#6891=AXIS2_PLACEMENT_3D('',#10852,#8177,#8178);
#6892=AXIS2_PLACEMENT_3D('',#10854,#8179,#8180);
#6893=AXIS2_PLACEMENT_3D('',#10855,#8181,#8182);
#6894=AXIS2_PLACEMENT_3D('',#10857,#8183,#8184);
#6895=AXIS2_PLACEMENT_3D('',#10859,#8186,#8187);
#6896=AXIS2_PLACEMENT_3D('',#10861,#8188,#8189);
#6897=AXIS2_PLACEMENT_3D('',#10864,#8191,#8192);
#6898=AXIS2_PLACEMENT_3D('',#10865,#8193,#8194);
#6899=AXIS2_PLACEMENT_3D('',#10866,#8195,#8196);
#6900=AXIS2_PLACEMENT_3D('',#10867,#8197,#8198);
#6901=AXIS2_PLACEMENT_3D('',#10868,#8199,#8200);
#6902=AXIS2_PLACEMENT_3D('',#10870,#8201,#8202);
#6903=AXIS2_PLACEMENT_3D('',#10873,#8204,#8205);
#6904=AXIS2_PLACEMENT_3D('',#10874,#8206,#8207);
#6905=AXIS2_PLACEMENT_3D('',#10876,#8208,#8209);
#6906=AXIS2_PLACEMENT_3D('',#10879,#8211,#8212);
#6907=AXIS2_PLACEMENT_3D('',#10880,#8213,#8214);
#6908=AXIS2_PLACEMENT_3D('',#10882,#8215,#8216);
#6909=AXIS2_PLACEMENT_3D('',#10885,#8218,#8219);
#6910=AXIS2_PLACEMENT_3D('',#10886,#8220,#8221);
#6911=AXIS2_PLACEMENT_3D('',#10888,#8222,#8223);
#6912=AXIS2_PLACEMENT_3D('',#10891,#8225,#8226);
#6913=AXIS2_PLACEMENT_3D('',#10892,#8227,#8228);
#6914=AXIS2_PLACEMENT_3D('',#10894,#8229,#8230);
#6915=AXIS2_PLACEMENT_3D('',#10897,#8232,#8233);
#6916=AXIS2_PLACEMENT_3D('',#10898,#8234,#8235);
#6917=AXIS2_PLACEMENT_3D('',#10900,#8236,#8237);
#6918=AXIS2_PLACEMENT_3D('',#10901,#8238,#8239);
#6919=AXIS2_PLACEMENT_3D('',#10904,#8241,#8242);
#6920=AXIS2_PLACEMENT_3D('',#10905,#8243,#8244);
#6921=AXIS2_PLACEMENT_3D('',#10907,#8245,#8246);
#6922=AXIS2_PLACEMENT_3D('',#10910,#8248,#8249);
#6923=AXIS2_PLACEMENT_3D('',#10911,#8250,#8251);
#6924=AXIS2_PLACEMENT_3D('',#10912,#8252,#8253);
#6925=AXIS2_PLACEMENT_3D('',#10913,#8254,#8255);
#6926=AXIS2_PLACEMENT_3D('',#10914,#8256,#8257);
#6927=AXIS2_PLACEMENT_3D('',#10916,#8258,#8259);
#6928=AXIS2_PLACEMENT_3D('',#10919,#8261,#8262);
#6929=AXIS2_PLACEMENT_3D('',#10920,#8263,#8264);
#6930=AXIS2_PLACEMENT_3D('',#10922,#8265,#8266);
#6931=AXIS2_PLACEMENT_3D('',#10925,#8268,#8269);
#6932=AXIS2_PLACEMENT_3D('',#10926,#8270,#8271);
#6933=AXIS2_PLACEMENT_3D('',#10928,#8272,#8273);
#6934=AXIS2_PLACEMENT_3D('',#10931,#8275,#8276);
#6935=AXIS2_PLACEMENT_3D('',#10932,#8277,#8278);
#6936=AXIS2_PLACEMENT_3D('',#10934,#8279,#8280);
#6937=AXIS2_PLACEMENT_3D('',#10937,#8282,#8283);
#6938=AXIS2_PLACEMENT_3D('',#10938,#8284,#8285);
#6939=AXIS2_PLACEMENT_3D('',#10940,#8286,#8287);
#6940=AXIS2_PLACEMENT_3D('',#10943,#8289,#8290);
#6941=AXIS2_PLACEMENT_3D('',#10944,#8291,#8292);
#6942=AXIS2_PLACEMENT_3D('',#10946,#8293,#8294);
#6943=AXIS2_PLACEMENT_3D('',#10947,#8295,#8296);
#6944=AXIS2_PLACEMENT_3D('',#10949,#8297,#8298);
#6945=AXIS2_PLACEMENT_3D('',#10951,#8300,#8301);
#6946=AXIS2_PLACEMENT_3D('',#10953,#8302,#8303);
#6947=AXIS2_PLACEMENT_3D('',#10956,#8305,#8306);
#6948=AXIS2_PLACEMENT_3D('',#10957,#8307,#8308);
#6949=AXIS2_PLACEMENT_3D('',#10958,#8309,#8310);
#6950=AXIS2_PLACEMENT_3D('',#10959,#8311,#8312);
#6951=AXIS2_PLACEMENT_3D('',#10960,#8313,#8314);
#6952=AXIS2_PLACEMENT_3D('',#11041,#8316,#8317);
#6953=AXIS2_PLACEMENT_3D('',#11043,#8318,#8319);
#6954=AXIS2_PLACEMENT_3D('',#11048,#8322,#8323);
#6955=AXIS2_PLACEMENT_3D('',#11050,#8324,#8325);
#6956=AXIS2_PLACEMENT_3D('',#11051,#8326,#8327);
#6957=AXIS2_PLACEMENT_3D('',#11052,#8328,#8329);
#6958=AXIS2_PLACEMENT_3D('',#11053,#8330,#8331);
#6959=AXIS2_PLACEMENT_3D('',#11057,#8334,#8335);
#6960=AXIS2_PLACEMENT_3D('',#11061,#8338,#8339);
#6961=AXIS2_PLACEMENT_3D('',#11067,#8343,#8344);
#6962=AXIS2_PLACEMENT_3D('',#11073,#8348,#8349);
#6963=AXIS2_PLACEMENT_3D('',#11077,#8352,#8353);
#6964=AXIS2_PLACEMENT_3D('',#11081,#8356,#8357);
#6965=AXIS2_PLACEMENT_3D('',#11083,#8359,#8360);
#6966=AXIS2_PLACEMENT_3D('',#11084,#8361,#8362);
#6967=AXIS2_PLACEMENT_3D('',#11085,#8363,#8364);
#6968=AXIS2_PLACEMENT_3D('',#11086,#8365,#8366);
#6969=AXIS2_PLACEMENT_3D('',#11089,#8367,#8368);
#6970=AXIS2_PLACEMENT_3D('',#11090,#8369,#8370);
#6971=AXIS2_PLACEMENT_3D('',#11092,#8371,#8372);
#6972=AXIS2_PLACEMENT_3D('',#11094,#8373,#8374);
#6973=AXIS2_PLACEMENT_3D('',#11095,#8375,#8376);
#6974=AXIS2_PLACEMENT_3D('',#11096,#8377,#8378);
#6975=AXIS2_PLACEMENT_3D('',#11099,#8380,#8381);
#6976=AXIS2_PLACEMENT_3D('',#11100,#8382,#8383);
#6977=AXIS2_PLACEMENT_3D('',#11102,#8384,#8385);
#6978=AXIS2_PLACEMENT_3D('',#11105,#8387,#8388);
#6979=AXIS2_PLACEMENT_3D('',#11106,#8389,#8390);
#6980=AXIS2_PLACEMENT_3D('',#11109,#8392,#8393);
#6981=AXIS2_PLACEMENT_3D('',#11110,#8394,#8395);
#6982=AXIS2_PLACEMENT_3D('',#11111,#8396,#8397);
#6983=AXIS2_PLACEMENT_3D('',#11113,#8398,#8399);
#6984=AXIS2_PLACEMENT_3D('',#11115,#8401,#8402);
#6985=AXIS2_PLACEMENT_3D('',#11117,#8403,#8404);
#6986=AXIS2_PLACEMENT_3D('',#11118,#8405,#8406);
#6987=AXIS2_PLACEMENT_3D('',#11120,#8408,#8409);
#6988=AXIS2_PLACEMENT_3D('',#11121,#8410,#8411);
#6989=AXIS2_PLACEMENT_3D('',#11124,#8412,#8413);
#6990=AXIS2_PLACEMENT_3D('',#11125,#8414,#8415);
#6991=AXIS2_PLACEMENT_3D('',#11127,#8416,#8417);
#6992=AXIS2_PLACEMENT_3D('',#11129,#8418,#8419);
#6993=AXIS2_PLACEMENT_3D('',#11130,#8420,#8421);
#6994=AXIS2_PLACEMENT_3D('',#11131,#8422,#8423);
#6995=AXIS2_PLACEMENT_3D('',#11133,#8424,#8425);
#6996=AXIS2_PLACEMENT_3D('',#11135,#8427,#8428);
#6997=AXIS2_PLACEMENT_3D('',#11137,#8429,#8430);
#6998=AXIS2_PLACEMENT_3D('',#11139,#8431,#8432);
#6999=AXIS2_PLACEMENT_3D('',#11140,#8433,#8434);
#7000=AXIS2_PLACEMENT_3D('',#11142,#8435,#8436);
#7001=AXIS2_PLACEMENT_3D('',#11144,#8438,#8439);
#7002=AXIS2_PLACEMENT_3D('',#11146,#8440,#8441);
#7003=AXIS2_PLACEMENT_3D('',#11148,#8443,#8444);
#7004=AXIS2_PLACEMENT_3D('',#11150,#8445,#8446);
#7005=AXIS2_PLACEMENT_3D('',#11152,#8448,#8449);
#7006=AXIS2_PLACEMENT_3D('',#11153,#8450,#8451);
#7007=AXIS2_PLACEMENT_3D('',#11155,#8453,#8454);
#7008=AXIS2_PLACEMENT_3D('',#11156,#8455,#8456);
#7009=AXIS2_PLACEMENT_3D('',#11159,#8457,#8458);
#7010=AXIS2_PLACEMENT_3D('',#11160,#8459,#8460);
#7011=AXIS2_PLACEMENT_3D('',#11163,#8461,#8462);
#7012=AXIS2_PLACEMENT_3D('',#11164,#8463,#8464);
#7013=AXIS2_PLACEMENT_3D('',#11167,#8465,#8466);
#7014=AXIS2_PLACEMENT_3D('',#11168,#8467,#8468);
#7015=AXIS2_PLACEMENT_3D('',#11171,#8469,#8470);
#7016=AXIS2_PLACEMENT_3D('',#11172,#8471,#8472);
#7017=AXIS2_PLACEMENT_3D('',#11175,#8473,#8474);
#7018=AXIS2_PLACEMENT_3D('',#11176,#8475,#8476);
#7019=AXIS2_PLACEMENT_3D('',#11179,#8477,#8478);
#7020=AXIS2_PLACEMENT_3D('',#11180,#8479,#8480);
#7021=AXIS2_PLACEMENT_3D('',#11183,#8481,#8482);
#7022=AXIS2_PLACEMENT_3D('',#11184,#8483,#8484);
#7023=AXIS2_PLACEMENT_3D('',#11187,#8485,#8486);
#7024=AXIS2_PLACEMENT_3D('',#11188,#8487,#8488);
#7025=AXIS2_PLACEMENT_3D('',#11189,#8489,#8490);
#7026=AXIS2_PLACEMENT_3D('',#11215,#8491,#8492);
#7027=AXIS2_PLACEMENT_3D('',#11239,#8493,#8494);
#7028=AXIS2_PLACEMENT_3D('',#11240,#8495,#8496);
#7029=AXIS2_PLACEMENT_3D('',#11242,#8497,#8498);
#7030=AXIS2_PLACEMENT_3D('',#11267,#8499,#8500);
#7031=AXIS2_PLACEMENT_3D('',#11292,#8501,#8502);
#7032=AXIS2_PLACEMENT_3D('',#11308,#8504,#8505);
#7033=AXIS2_PLACEMENT_3D('',#11323,#8506,#8507);
#7034=AXIS2_PLACEMENT_3D('',#11348,#8508,#8509);
#7035=AXIS2_PLACEMENT_3D('',#11373,#8510,#8511);
#7036=AXIS2_PLACEMENT_3D('',#11398,#8512,#8513);
#7037=AXIS2_PLACEMENT_3D('',#11422,#8514,#8515);
#7038=AXIS2_PLACEMENT_3D('',#11423,#8516,#8517);
#7039=AXIS2_PLACEMENT_3D('',#11425,#8518,#8519);
#7040=AXIS2_PLACEMENT_3D('',#11426,#8520,#8521);
#7041=AXIS2_PLACEMENT_3D('',#11427,#8522,#8523);
#7042=AXIS2_PLACEMENT_3D('',#11451,#8524,#8525);
#7043=AXIS2_PLACEMENT_3D('',#11452,#8526,#8527);
#7044=AXIS2_PLACEMENT_3D('',#11454,#8528,#8529);
#7045=AXIS2_PLACEMENT_3D('',#11455,#8530,#8531);
#7046=AXIS2_PLACEMENT_3D('',#11456,#8532,#8533);
#7047=AXIS2_PLACEMENT_3D('',#11480,#8534,#8535);
#7048=AXIS2_PLACEMENT_3D('',#11481,#8536,#8537);
#7049=AXIS2_PLACEMENT_3D('',#11483,#8538,#8539);
#7050=AXIS2_PLACEMENT_3D('',#11484,#8540,#8541);
#7051=AXIS2_PLACEMENT_3D('',#11485,#8542,#8543);
#7052=AXIS2_PLACEMENT_3D('',#11500,#8544,#8545);
#7053=AXIS2_PLACEMENT_3D('',#11513,#8546,#8547);
#7054=AXIS2_PLACEMENT_3D('',#11515,#8548,#8549);
#7055=AXIS2_PLACEMENT_3D('',#11516,#8550,#8551);
#7056=AXIS2_PLACEMENT_3D('',#11517,#8552,#8553);
#7057=AXIS2_PLACEMENT_3D('',#11541,#8554,#8555);
#7058=AXIS2_PLACEMENT_3D('',#11542,#8556,#8557);
#7059=AXIS2_PLACEMENT_3D('',#11544,#8558,#8559);
#7060=AXIS2_PLACEMENT_3D('',#11545,#8560,#8561);
#7061=AXIS2_PLACEMENT_3D('',#11546,#8562,#8563);
#7062=AXIS2_PLACEMENT_3D('',#11570,#8564,#8565);
#7063=AXIS2_PLACEMENT_3D('',#11571,#8566,#8567);
#7064=AXIS2_PLACEMENT_3D('',#11573,#8568,#8569);
#7065=AXIS2_PLACEMENT_3D('',#11574,#8570,#8571);
#7066=AXIS2_PLACEMENT_3D('',#11575,#8572,#8573);
#7067=AXIS2_PLACEMENT_3D('',#11599,#8574,#8575);
#7068=AXIS2_PLACEMENT_3D('',#11600,#8576,#8577);
#7069=AXIS2_PLACEMENT_3D('',#11602,#8578,#8579);
#7070=AXIS2_PLACEMENT_3D('',#11605,#8581,#8582);
#7071=AXIS2_PLACEMENT_3D('',#11629,#8583,#8584);
#7072=AXIS2_PLACEMENT_3D('',#11630,#8585,#8586);
#7073=AXIS2_PLACEMENT_3D('',#11631,#8587,#8588);
#7074=AXIS2_PLACEMENT_3D('',#11632,#8589,#8590);
#7075=AXIS2_PLACEMENT_3D('',#11633,#8591,#8592);
#7076=AXIS2_PLACEMENT_3D('',#11634,#8593,#8594);
#7077=AXIS2_PLACEMENT_3D('',#11635,#8595,#8596);
#7078=AXIS2_PLACEMENT_3D('',#11636,#8597,#8598);
#7079=AXIS2_PLACEMENT_3D('',#11637,#8599,#8600);
#7080=AXIS2_PLACEMENT_3D('',#11639,#8601,#8602);
#7081=AXIS2_PLACEMENT_3D('',#11641,#8603,#8604);
#7082=AXIS2_PLACEMENT_3D('',#11642,#8605,#8606);
#7083=AXIS2_PLACEMENT_3D('',#11644,#8607,#8608);
#7084=AXIS2_PLACEMENT_3D('',#11646,#8610,#8611);
#7085=AXIS2_PLACEMENT_3D('',#11648,#8612,#8613);
#7086=AXIS2_PLACEMENT_3D('',#11649,#8614,#8615);
#7087=AXIS2_PLACEMENT_3D('',#11651,#8617,#8618);
#7088=AXIS2_PLACEMENT_3D('',#11653,#8619,#8620);
#7089=AXIS2_PLACEMENT_3D('',#11655,#8621,#8622);
#7090=AXIS2_PLACEMENT_3D('',#11656,#8623,#8624);
#7091=AXIS2_PLACEMENT_3D('',#11658,#8625,#8626);
#7092=AXIS2_PLACEMENT_3D('',#11660,#8628,#8629);
#7093=AXIS2_PLACEMENT_3D('',#11662,#8630,#8631);
#7094=AXIS2_PLACEMENT_3D('',#11663,#8632,#8633);
#7095=AXIS2_PLACEMENT_3D('',#11665,#8635,#8636);
#7096=AXIS2_PLACEMENT_3D('',#11666,#8637,#8638);
#7097=AXIS2_PLACEMENT_3D('',#11667,#8639,#8640);
#7098=AXIS2_PLACEMENT_3D('',#11668,#8641,#8642);
#7099=AXIS2_PLACEMENT_3D('',#11669,#8643,#8644);
#7100=AXIS2_PLACEMENT_3D('',#11670,#8645,#8646);
#7101=AXIS2_PLACEMENT_3D('',#11671,#8647,#8648);
#7102=AXIS2_PLACEMENT_3D('',#11673,#8649,#8650);
#7103=AXIS2_PLACEMENT_3D('',#11674,#8651,#8652);
#7104=AXIS2_PLACEMENT_3D('',#11676,#8653,#8654);
#7105=AXIS2_PLACEMENT_3D('',#11677,#8655,#8656);
#7106=AXIS2_PLACEMENT_3D('',#11679,#8657,#8658);
#7107=AXIS2_PLACEMENT_3D('',#11681,#8660,#8661);
#7108=AXIS2_PLACEMENT_3D('',#11683,#8662,#8663);
#7109=AXIS2_PLACEMENT_3D('',#11685,#8665,#8666);
#7110=AXIS2_PLACEMENT_3D('',#11687,#8667,#8668);
#7111=AXIS2_PLACEMENT_3D('',#11689,#8670,#8671);
#7112=AXIS2_PLACEMENT_3D('',#11691,#8672,#8673);
#7113=AXIS2_PLACEMENT_3D('',#11692,#8674,#8675);
#7114=AXIS2_PLACEMENT_3D('',#11694,#8676,#8677);
#7115=AXIS2_PLACEMENT_3D('',#11696,#8679,#8680);
#7116=AXIS2_PLACEMENT_3D('',#11698,#8682,#8683);
#7117=AXIS2_PLACEMENT_3D('',#11707,#8688,#8689);
#7118=AXIS2_PLACEMENT_3D('',#11713,#8693,#8694);
#7119=AXIS2_PLACEMENT_3D('',#11719,#8698,#8699);
#7120=AXIS2_PLACEMENT_3D('',#11725,#8703,#8704);
#7121=AXIS2_PLACEMENT_3D('',#11731,#8708,#8709);
#7122=AXIS2_PLACEMENT_3D('',#11734,#8712,#8713);
#7123=AXIS2_PLACEMENT_3D('',#11735,#8714,#8715);
#7124=AXIS2_PLACEMENT_3D('',#11736,#8716,#8717);
#7125=AXIS2_PLACEMENT_3D('',#11737,#8718,#8719);
#7126=AXIS2_PLACEMENT_3D('',#11738,#8720,#8721);
#7127=AXIS2_PLACEMENT_3D('',#11739,#8722,#8723);
#7128=AXIS2_PLACEMENT_3D('',#11740,#8724,#8725);
#7129=AXIS2_PLACEMENT_3D('',#11741,#8726,#8727);
#7130=AXIS2_PLACEMENT_3D('',#11742,#8728,#8729);
#7131=AXIS2_PLACEMENT_3D('',#11743,#8730,#8731);
#7132=AXIS2_PLACEMENT_3D('',#11744,#8732,#8733);
#7133=AXIS2_PLACEMENT_3D('',#11745,#8734,#8735);
#7134=AXIS2_PLACEMENT_3D('',#11746,#8736,#8737);
#7135=AXIS2_PLACEMENT_3D('',#11747,#8738,#8739);
#7136=AXIS2_PLACEMENT_3D('',#11748,#8740,#8741);
#7137=AXIS2_PLACEMENT_3D('',#11749,#8742,#8743);
#7138=AXIS2_PLACEMENT_3D('',#11750,#8744,#8745);
#7139=AXIS2_PLACEMENT_3D('',#11751,#8746,#8747);
#7140=AXIS2_PLACEMENT_3D('',#11752,#8748,#8749);
#7141=AXIS2_PLACEMENT_3D('',#11753,#8750,#8751);
#7142=AXIS2_PLACEMENT_3D('',#11754,#8752,#8753);
#7143=AXIS2_PLACEMENT_3D('',#11755,#8754,#8755);
#7144=AXIS2_PLACEMENT_3D('',#11756,#8756,#8757);
#7145=AXIS2_PLACEMENT_3D('',#11757,#8758,#8759);
#7146=AXIS2_PLACEMENT_3D('',#11758,#8760,#8761);
#7147=AXIS2_PLACEMENT_3D('',#11759,#8762,#8763);
#7148=AXIS2_PLACEMENT_3D('',#11760,#8764,#8765);
#7149=AXIS2_PLACEMENT_3D('',#11761,#8766,#8767);
#7150=AXIS2_PLACEMENT_3D('',#11762,#8768,#8769);
#7151=AXIS2_PLACEMENT_3D('',#11764,#8770,#8771);
#7152=AXIS2_PLACEMENT_3D('',#11767,#8773,#8774);
#7153=AXIS2_PLACEMENT_3D('',#11768,#8775,#8776);
#7154=AXIS2_PLACEMENT_3D('',#11769,#8777,#8778);
#7155=AXIS2_PLACEMENT_3D('',#11771,#8779,#8780);
#7156=AXIS2_PLACEMENT_3D('',#11774,#8782,#8783);
#7157=AXIS2_PLACEMENT_3D('',#11775,#8784,#8785);
#7158=AXIS2_PLACEMENT_3D('',#11776,#8786,#8787);
#7159=AXIS2_PLACEMENT_3D('',#11778,#8788,#8789);
#7160=AXIS2_PLACEMENT_3D('',#11780,#8790,#8791);
#7161=AXIS2_PLACEMENT_3D('',#11781,#8792,#8793);
#7162=AXIS2_PLACEMENT_3D('',#11783,#8794,#8795);
#7163=AXIS2_PLACEMENT_3D('',#11785,#8797,#8798);
#7164=AXIS2_PLACEMENT_3D('',#11788,#8800,#8801);
#7165=AXIS2_PLACEMENT_3D('',#11789,#8802,#8803);
#7166=AXIS2_PLACEMENT_3D('',#11790,#8804,#8805);
#7167=AXIS2_PLACEMENT_3D('',#11791,#8806,#8807);
#7168=AXIS2_PLACEMENT_3D('',#11792,#8808,#8809);
#7169=AXIS2_PLACEMENT_3D('',#11796,#8811,#8812);
#7170=AXIS2_PLACEMENT_3D('',#11797,#8813,#8814);
#7171=AXIS2_PLACEMENT_3D('',#11814,#8815,#8816);
#7172=AXIS2_PLACEMENT_3D('',#11871,#8818,#8819);
#7173=AXIS2_PLACEMENT_3D('',#11873,#8821,#8822);
#7174=AXIS2_PLACEMENT_3D('',#11875,#8823,#8824);
#7175=AXIS2_PLACEMENT_3D('',#11878,#8826,#8827);
#7176=AXIS2_PLACEMENT_3D('',#11879,#8828,#8829);
#7177=AXIS2_PLACEMENT_3D('',#11881,#8830,#8831);
#7178=AXIS2_PLACEMENT_3D('',#11884,#8833,#8834);
#7179=AXIS2_PLACEMENT_3D('',#11885,#8835,#8836);
#7180=AXIS2_PLACEMENT_3D('',#11886,#8837,#8838);
#7181=AXIS2_PLACEMENT_3D('',#11887,#8839,#8840);
#7182=AXIS2_PLACEMENT_3D('',#11888,#8841,#8842);
#7183=AXIS2_PLACEMENT_3D('',#11890,#8843,#8844);
#7184=AXIS2_PLACEMENT_3D('',#11893,#8846,#8847);
#7185=AXIS2_PLACEMENT_3D('',#11894,#8848,#8849);
#7186=AXIS2_PLACEMENT_3D('',#11896,#8850,#8851);
#7187=AXIS2_PLACEMENT_3D('',#11899,#8853,#8854);
#7188=AXIS2_PLACEMENT_3D('',#11900,#8855,#8856);
#7189=AXIS2_PLACEMENT_3D('',#11901,#8857,#8858);
#7190=AXIS2_PLACEMENT_3D('',#11902,#8859,#8860);
#7191=AXIS2_PLACEMENT_3D('',#11903,#8861,#8862);
#7192=AXIS2_PLACEMENT_3D('',#11905,#8863,#8864);
#7193=AXIS2_PLACEMENT_3D('',#11908,#8866,#8867);
#7194=AXIS2_PLACEMENT_3D('',#11909,#8868,#8869);
#7195=AXIS2_PLACEMENT_3D('',#11911,#8870,#8871);
#7196=AXIS2_PLACEMENT_3D('',#11914,#8873,#8874);
#7197=AXIS2_PLACEMENT_3D('',#11915,#8875,#8876);
#7198=AXIS2_PLACEMENT_3D('',#11916,#8877,#8878);
#7199=AXIS2_PLACEMENT_3D('',#11917,#8879,#8880);
#7200=AXIS2_PLACEMENT_3D('',#11918,#8881,#8882);
#7201=AXIS2_PLACEMENT_3D('',#11920,#8883,#8884);
#7202=AXIS2_PLACEMENT_3D('',#11923,#8886,#8887);
#7203=AXIS2_PLACEMENT_3D('',#11924,#8888,#8889);
#7204=AXIS2_PLACEMENT_3D('',#11925,#8890,#8891);
#7205=AXIS2_PLACEMENT_3D('',#11926,#8892,#8893);
#7206=AXIS2_PLACEMENT_3D('',#11927,#8894,#8895);
#7207=AXIS2_PLACEMENT_3D('',#11929,#8896,#8897);
#7208=AXIS2_PLACEMENT_3D('',#11932,#8899,#8900);
#7209=AXIS2_PLACEMENT_3D('',#11933,#8901,#8902);
#7210=AXIS2_PLACEMENT_3D('',#11934,#8903,#8904);
#7211=AXIS2_PLACEMENT_3D('',#11935,#8905,#8906);
#7212=AXIS2_PLACEMENT_3D('',#11936,#8907,#8908);
#7213=AXIS2_PLACEMENT_3D('',#11938,#8909,#8910);
#7214=AXIS2_PLACEMENT_3D('',#11941,#8912,#8913);
#7215=AXIS2_PLACEMENT_3D('',#11942,#8914,#8915);
#7216=AXIS2_PLACEMENT_3D('',#11944,#8916,#8917);
#7217=AXIS2_PLACEMENT_3D('',#11947,#8919,#8920);
#7218=AXIS2_PLACEMENT_3D('',#11948,#8921,#8922);
#7219=AXIS2_PLACEMENT_3D('',#11949,#8923,#8924);
#7220=AXIS2_PLACEMENT_3D('',#11950,#8925,#8926);
#7221=AXIS2_PLACEMENT_3D('',#11951,#8927,#8928);
#7222=AXIS2_PLACEMENT_3D('',#11953,#8929,#8930);
#7223=AXIS2_PLACEMENT_3D('',#11954,#8931,#8932);
#7224=AXIS2_PLACEMENT_3D('',#11963,#8937,#8938);
#7225=AXIS2_PLACEMENT_3D('',#11969,#8942,#8943);
#7226=AXIS2_PLACEMENT_3D('',#11975,#8947,#8948);
#7227=AXIS2_PLACEMENT_3D('',#11981,#8952,#8953);
#7228=AXIS2_PLACEMENT_3D('',#11987,#8957,#8958);
#7229=AXIS2_PLACEMENT_3D('',#11990,#8961,#8962);
#7230=AXIS2_PLACEMENT_3D('',#11991,#8963,#8964);
#7231=AXIS2_PLACEMENT_3D('',#11993,#8965,#8966);
#7232=AXIS2_PLACEMENT_3D('',#11994,#8967,#8968);
#7233=AXIS2_PLACEMENT_3D('',#11996,#8969,#8970);
#7234=AXIS2_PLACEMENT_3D('',#11998,#8972,#8973);
#7235=AXIS2_PLACEMENT_3D('',#12000,#8975,#8976);
#7236=AXIS2_PLACEMENT_3D('',#12001,#8977,#8978);
#7237=AXIS2_PLACEMENT_3D('',#12002,#8979,#8980);
#7238=AXIS2_PLACEMENT_3D('',#12003,#8981,#8982);
#7239=AXIS2_PLACEMENT_3D('',#12004,#8983,#8984);
#7240=AXIS2_PLACEMENT_3D('',#12005,#8985,#8986);
#7241=AXIS2_PLACEMENT_3D('',#12006,#8987,#8988);
#7242=AXIS2_PLACEMENT_3D('',#12007,#8989,#8990);
#7243=AXIS2_PLACEMENT_3D('',#12008,#8991,#8992);
#7244=AXIS2_PLACEMENT_3D('',#12009,#8993,#8994);
#7245=AXIS2_PLACEMENT_3D('',#12010,#8995,#8996);
#7246=AXIS2_PLACEMENT_3D('',#12011,#8997,#8998);
#7247=AXIS2_PLACEMENT_3D('',#12012,#8999,#9000);
#7248=AXIS2_PLACEMENT_3D('',#12013,#9001,#9002);
#7249=AXIS2_PLACEMENT_3D('',#12014,#9003,#9004);
#7250=AXIS2_PLACEMENT_3D('',#12015,#9005,#9006);
#7251=AXIS2_PLACEMENT_3D('',#12016,#9007,#9008);
#7252=AXIS2_PLACEMENT_3D('',#12017,#9009,#9010);
#7253=AXIS2_PLACEMENT_3D('',#12018,#9011,#9012);
#7254=AXIS2_PLACEMENT_3D('',#12019,#9013,#9014);
#7255=AXIS2_PLACEMENT_3D('',#12020,#9015,#9016);
#7256=AXIS2_PLACEMENT_3D('',#12107,#9018,#9019);
#7257=AXIS2_PLACEMENT_3D('',#12188,#9021,#9022);
#7258=AXIS2_PLACEMENT_3D('',#12190,#9023,#9024);
#7259=AXIS2_PLACEMENT_3D('',#12194,#9027,#9028);
#7260=AXIS2_PLACEMENT_3D('',#12277,#9029,#9030);
#7261=AXIS2_PLACEMENT_3D('',#12317,#9032,#9033);
#7262=AXIS2_PLACEMENT_3D('',#12357,#9035,#9036);
#7263=AXIS2_PLACEMENT_3D('',#12359,#9037,#9038);
#7264=AXIS2_PLACEMENT_3D('',#12363,#9041,#9042);
#7265=AXIS2_PLACEMENT_3D('',#12364,#9043,#9044);
#7266=AXIS2_PLACEMENT_3D('',#12365,#9045,#9046);
#7267=AXIS2_PLACEMENT_3D('',#12367,#9047,#9048);
#7268=AXIS2_PLACEMENT_3D('',#12370,#9049,#9050);
#7269=AXIS2_PLACEMENT_3D('',#12372,#9051,#9052);
#7270=AXIS2_PLACEMENT_3D('',#12374,#9053,#9054);
#7271=AXIS2_PLACEMENT_3D('',#12376,#9055,#9056);
#7272=AXIS2_PLACEMENT_3D('',#12378,#9057,#9058);
#7273=AXIS2_PLACEMENT_3D('',#12380,#9059,#9060);
#7274=AXIS2_PLACEMENT_3D('',#12382,#9061,#9062);
#7275=AXIS2_PLACEMENT_3D('',#12384,#9063,#9064);
#7276=AXIS2_PLACEMENT_3D('',#12386,#9065,#9066);
#7277=AXIS2_PLACEMENT_3D('',#12388,#9067,#9068);
#7278=AXIS2_PLACEMENT_3D('',#12390,#9069,#9070);
#7279=AXIS2_PLACEMENT_3D('',#12392,#9071,#9072);
#7280=AXIS2_PLACEMENT_3D('',#12394,#9073,#9074);
#7281=AXIS2_PLACEMENT_3D('',#12396,#9075,#9076);
#7282=AXIS2_PLACEMENT_3D('',#12398,#9077,#9078);
#7283=AXIS2_PLACEMENT_3D('',#12400,#9079,#9080);
#7284=AXIS2_PLACEMENT_3D('',#12402,#9081,#9082);
#7285=AXIS2_PLACEMENT_3D('',#12404,#9083,#9084);
#7286=AXIS2_PLACEMENT_3D('',#12406,#9085,#9086);
#7287=AXIS2_PLACEMENT_3D('',#12408,#9087,#9088);
#7288=AXIS2_PLACEMENT_3D('',#12410,#9089,#9090);
#7289=AXIS2_PLACEMENT_3D('',#12412,#9091,#9092);
#7290=AXIS2_PLACEMENT_3D('',#12414,#9093,#9094);
#7291=AXIS2_PLACEMENT_3D('',#12416,#9095,#9096);
#7292=AXIS2_PLACEMENT_3D('',#12418,#9097,#9098);
#7293=AXIS2_PLACEMENT_3D('',#12420,#9099,#9100);
#7294=AXIS2_PLACEMENT_3D('',#12422,#9101,#9102);
#7295=AXIS2_PLACEMENT_3D('',#12424,#9103,#9104);
#7296=AXIS2_PLACEMENT_3D('',#12426,#9105,#9106);
#7297=AXIS2_PLACEMENT_3D('',#12428,#9107,#9108);
#7298=AXIS2_PLACEMENT_3D('',#12430,#9109,#9110);
#7299=AXIS2_PLACEMENT_3D('',#12432,#9111,#9112);
#7300=AXIS2_PLACEMENT_3D('',#12434,#9113,#9114);
#7301=AXIS2_PLACEMENT_3D('',#12436,#9115,#9116);
#7302=AXIS2_PLACEMENT_3D('',#12438,#9117,#9118);
#7303=AXIS2_PLACEMENT_3D('',#12440,#9119,#9120);
#7304=AXIS2_PLACEMENT_3D('',#12442,#9121,#9122);
#7305=AXIS2_PLACEMENT_3D('',#12444,#9123,#9124);
#7306=AXIS2_PLACEMENT_3D('',#12446,#9125,#9126);
#7307=AXIS2_PLACEMENT_3D('',#12447,#9127,#9128);
#7308=AXIS2_PLACEMENT_3D('',#12448,#9129,#9130);
#7309=AXIS2_PLACEMENT_3D('',#12450,#9131,#9132);
#7310=AXIS2_PLACEMENT_3D('',#12452,#9134,#9135);
#7311=AXIS2_PLACEMENT_3D('',#12453,#9136,#9137);
#7312=AXIS2_PLACEMENT_3D('',#12455,#9138,#9139);
#7313=AXIS2_PLACEMENT_3D('',#12458,#9140,#9141);
#7314=AXIS2_PLACEMENT_3D('',#12460,#9142,#9143);
#7315=AXIS2_PLACEMENT_3D('',#12462,#9144,#9145);
#7316=AXIS2_PLACEMENT_3D('',#12464,#9146,#9147);
#7317=AXIS2_PLACEMENT_3D('',#12466,#9148,#9149);
#7318=AXIS2_PLACEMENT_3D('',#12468,#9150,#9151);
#7319=AXIS2_PLACEMENT_3D('',#12470,#9152,#9153);
#7320=AXIS2_PLACEMENT_3D('',#12472,#9154,#9155);
#7321=AXIS2_PLACEMENT_3D('',#12474,#9156,#9157);
#7322=AXIS2_PLACEMENT_3D('',#12476,#9158,#9159);
#7323=AXIS2_PLACEMENT_3D('',#12478,#9160,#9161);
#7324=AXIS2_PLACEMENT_3D('',#12480,#9162,#9163);
#7325=AXIS2_PLACEMENT_3D('',#12482,#9164,#9165);
#7326=AXIS2_PLACEMENT_3D('',#12484,#9166,#9167);
#7327=AXIS2_PLACEMENT_3D('',#12486,#9168,#9169);
#7328=AXIS2_PLACEMENT_3D('',#12488,#9170,#9171);
#7329=AXIS2_PLACEMENT_3D('',#12490,#9172,#9173);
#7330=AXIS2_PLACEMENT_3D('',#12492,#9174,#9175);
#7331=AXIS2_PLACEMENT_3D('',#12494,#9176,#9177);
#7332=AXIS2_PLACEMENT_3D('',#12496,#9178,#9179);
#7333=AXIS2_PLACEMENT_3D('',#12498,#9180,#9181);
#7334=AXIS2_PLACEMENT_3D('',#12500,#9182,#9183);
#7335=AXIS2_PLACEMENT_3D('',#12502,#9184,#9185);
#7336=AXIS2_PLACEMENT_3D('',#12504,#9186,#9187);
#7337=AXIS2_PLACEMENT_3D('',#12506,#9188,#9189);
#7338=AXIS2_PLACEMENT_3D('',#12508,#9190,#9191);
#7339=AXIS2_PLACEMENT_3D('',#12510,#9192,#9193);
#7340=AXIS2_PLACEMENT_3D('',#12512,#9194,#9195);
#7341=AXIS2_PLACEMENT_3D('',#12514,#9196,#9197);
#7342=AXIS2_PLACEMENT_3D('',#12516,#9198,#9199);
#7343=AXIS2_PLACEMENT_3D('',#12518,#9200,#9201);
#7344=AXIS2_PLACEMENT_3D('',#12520,#9202,#9203);
#7345=AXIS2_PLACEMENT_3D('',#12522,#9204,#9205);
#7346=AXIS2_PLACEMENT_3D('',#12524,#9206,#9207);
#7347=AXIS2_PLACEMENT_3D('',#12526,#9208,#9209);
#7348=AXIS2_PLACEMENT_3D('',#12528,#9210,#9211);
#7349=AXIS2_PLACEMENT_3D('',#12530,#9212,#9213);
#7350=AXIS2_PLACEMENT_3D('',#12532,#9214,#9215);
#7351=AXIS2_PLACEMENT_3D('',#12534,#9216,#9217);
#7352=AXIS2_PLACEMENT_3D('',#12535,#9218,#9219);
#7353=AXIS2_PLACEMENT_3D('',#12536,#9220,#9221);
#7354=AXIS2_PLACEMENT_3D('',#12538,#9222,#9223);
#7355=AXIS2_PLACEMENT_3D('',#12540,#9225,#9226);
#7356=AXIS2_PLACEMENT_3D('',#12541,#9227,#9228);
#7357=AXIS2_PLACEMENT_3D('',#12544,#9231,#9232);
#7358=AXIS2_PLACEMENT_3D('',#12546,#9234,#9235);
#7359=AXIS2_PLACEMENT_3D('',#12548,#9237,#9238);
#7360=AXIS2_PLACEMENT_3D('',#12550,#9240,#9241);
#7361=AXIS2_PLACEMENT_3D('',#12552,#9243,#9244);
#7362=AXIS2_PLACEMENT_3D('',#12554,#9246,#9247);
#7363=AXIS2_PLACEMENT_3D('',#12556,#9249,#9250);
#7364=AXIS2_PLACEMENT_3D('',#12558,#9252,#9253);
#7365=AXIS2_PLACEMENT_3D('',#12560,#9255,#9256);
#7366=AXIS2_PLACEMENT_3D('',#12562,#9258,#9259);
#7367=AXIS2_PLACEMENT_3D('',#12564,#9261,#9262);
#7368=AXIS2_PLACEMENT_3D('',#12566,#9264,#9265);
#7369=AXIS2_PLACEMENT_3D('',#12568,#9267,#9268);
#7370=AXIS2_PLACEMENT_3D('',#12570,#9270,#9271);
#7371=AXIS2_PLACEMENT_3D('',#12572,#9273,#9274);
#7372=AXIS2_PLACEMENT_3D('',#12574,#9276,#9277);
#7373=AXIS2_PLACEMENT_3D('',#12576,#9279,#9280);
#7374=AXIS2_PLACEMENT_3D('',#12578,#9282,#9283);
#7375=AXIS2_PLACEMENT_3D('',#12580,#9285,#9286);
#7376=AXIS2_PLACEMENT_3D('',#12582,#9288,#9289);
#7377=AXIS2_PLACEMENT_3D('',#12584,#9291,#9292);
#7378=AXIS2_PLACEMENT_3D('',#12586,#9294,#9295);
#7379=AXIS2_PLACEMENT_3D('',#12588,#9297,#9298);
#7380=AXIS2_PLACEMENT_3D('',#12590,#9300,#9301);
#7381=AXIS2_PLACEMENT_3D('',#12592,#9303,#9304);
#7382=AXIS2_PLACEMENT_3D('',#12594,#9306,#9307);
#7383=AXIS2_PLACEMENT_3D('',#12596,#9309,#9310);
#7384=AXIS2_PLACEMENT_3D('',#12598,#9312,#9313);
#7385=AXIS2_PLACEMENT_3D('',#12600,#9315,#9316);
#7386=AXIS2_PLACEMENT_3D('',#12602,#9318,#9319);
#7387=AXIS2_PLACEMENT_3D('',#12604,#9321,#9322);
#7388=AXIS2_PLACEMENT_3D('',#12606,#9324,#9325);
#7389=AXIS2_PLACEMENT_3D('',#12608,#9327,#9328);
#7390=AXIS2_PLACEMENT_3D('',#12610,#9330,#9331);
#7391=AXIS2_PLACEMENT_3D('',#12612,#9333,#9334);
#7392=AXIS2_PLACEMENT_3D('',#12614,#9336,#9337);
#7393=AXIS2_PLACEMENT_3D('',#12616,#9339,#9340);
#7394=AXIS2_PLACEMENT_3D('',#12618,#9342,#9343);
#7395=AXIS2_PLACEMENT_3D('',#12620,#9345,#9346);
#7396=AXIS2_PLACEMENT_3D('',#12621,#9347,#9348);
#7397=AXIS2_PLACEMENT_3D('',#12622,#9349,#9350);
#7398=AXIS2_PLACEMENT_3D('',#12631,#9355,#9356);
#7399=AXIS2_PLACEMENT_3D('',#12637,#9360,#9361);
#7400=AXIS2_PLACEMENT_3D('',#12643,#9365,#9366);
#7401=AXIS2_PLACEMENT_3D('',#12649,#9370,#9371);
#7402=AXIS2_PLACEMENT_3D('',#12655,#9375,#9376);
#7403=AXIS2_PLACEMENT_3D('',#12658,#9379,#9380);
#7404=AXIS2_PLACEMENT_3D('',#12659,#9381,#9382);
#7405=AXIS2_PLACEMENT_3D('',#12660,#9383,#9384);
#7406=AXIS2_PLACEMENT_3D('',#12662,#9385,#9386);
#7407=AXIS2_PLACEMENT_3D('',#12663,#9387,#9388);
#7408=AXIS2_PLACEMENT_3D('',#12665,#9389,#9390);
#7409=AXIS2_PLACEMENT_3D('',#12666,#9391,#9392);
#7410=AXIS2_PLACEMENT_3D('',#12668,#9393,#9394);
#7411=AXIS2_PLACEMENT_3D('',#12670,#9396,#9397);
#7412=AXIS2_PLACEMENT_3D('',#12672,#9398,#9399);
#7413=AXIS2_PLACEMENT_3D('',#12674,#9401,#9402);
#7414=AXIS2_PLACEMENT_3D('',#12676,#9403,#9404);
#7415=AXIS2_PLACEMENT_3D('',#12678,#9406,#9407);
#7416=AXIS2_PLACEMENT_3D('',#12680,#9408,#9409);
#7417=AXIS2_PLACEMENT_3D('',#12681,#9410,#9411);
#7418=AXIS2_PLACEMENT_3D('',#12683,#9412,#9413);
#7419=AXIS2_PLACEMENT_3D('',#12685,#9415,#9416);
#7420=AXIS2_PLACEMENT_3D('',#12687,#9418,#9419);
#7421=AXIS2_PLACEMENT_3D('',#12688,#9420,#9421);
#7422=AXIS2_PLACEMENT_3D('',#12689,#9422,#9423);
#7423=AXIS2_PLACEMENT_3D('',#12690,#9424,#9425);
#7424=AXIS2_PLACEMENT_3D('',#12691,#9426,#9427);
#7425=AXIS2_PLACEMENT_3D('',#12692,#9428,#9429);
#7426=AXIS2_PLACEMENT_3D('',#12693,#9430,#9431);
#7427=AXIS2_PLACEMENT_3D('',#12694,#9432,#9433);
#7428=AXIS2_PLACEMENT_3D('',#12695,#9434,#9435);
#7429=AXIS2_PLACEMENT_3D('',#12696,#9436,#9437);
#7430=AXIS2_PLACEMENT_3D('',#12697,#9438,#9439);
#7431=AXIS2_PLACEMENT_3D('',#12698,#9440,#9441);
#7432=AXIS2_PLACEMENT_3D('',#12699,#9442,#9443);
#7433=DIRECTION('axis',(0.,0.,1.));
#7434=DIRECTION('refdir',(1.,0.,0.));
#7435=DIRECTION('axis',(0.,0.,1.));
#7436=DIRECTION('refdir',(1.,0.,0.));
#7437=DIRECTION('axis',(0.,0.,1.));
#7438=DIRECTION('refdir',(1.,0.,0.));
#7439=DIRECTION('center_axis',(0.,0.,1.));
#7440=DIRECTION('ref_axis',(1.,0.,0.));
#7441=DIRECTION('center_axis',(0.,0.,1.));
#7442=DIRECTION('ref_axis',(1.,0.,0.));
#7443=DIRECTION('',(0.,0.,1.));
#7444=DIRECTION('center_axis',(0.,0.,-1.));
#7445=DIRECTION('ref_axis',(1.,0.,0.));
#7446=DIRECTION('center_axis',(0.,0.,1.));
#7447=DIRECTION('ref_axis',(1.,0.,0.));
#7448=DIRECTION('center_axis',(0.,0.,1.));
#7449=DIRECTION('ref_axis',(1.,0.,0.));
#7450=DIRECTION('',(0.,0.,1.));
#7451=DIRECTION('center_axis',(0.,0.,-1.));
#7452=DIRECTION('ref_axis',(1.,0.,0.));
#7453=DIRECTION('center_axis',(0.,0.,1.));
#7454=DIRECTION('ref_axis',(1.,0.,0.));
#7455=DIRECTION('center_axis',(0.,0.,1.));
#7456=DIRECTION('ref_axis',(1.,0.,0.));
#7457=DIRECTION('',(0.,0.,1.));
#7458=DIRECTION('center_axis',(0.,0.,-1.));
#7459=DIRECTION('ref_axis',(1.,0.,0.));
#7460=DIRECTION('center_axis',(0.,0.,1.));
#7461=DIRECTION('ref_axis',(1.,0.,0.));
#7462=DIRECTION('center_axis',(0.,0.,1.));
#7463=DIRECTION('ref_axis',(1.,0.,0.));
#7464=DIRECTION('',(0.,0.,1.));
#7465=DIRECTION('center_axis',(0.,0.,-1.));
#7466=DIRECTION('ref_axis',(1.,0.,0.));
#7467=DIRECTION('center_axis',(0.,0.,1.));
#7468=DIRECTION('ref_axis',(1.,0.,0.));
#7469=DIRECTION('center_axis',(0.,0.,1.));
#7470=DIRECTION('ref_axis',(1.,0.,0.));
#7471=DIRECTION('',(0.,0.,1.));
#7472=DIRECTION('center_axis',(0.,0.,-1.));
#7473=DIRECTION('ref_axis',(1.,0.,0.));
#7474=DIRECTION('center_axis',(0.,1.,0.));
#7475=DIRECTION('ref_axis',(-1.,0.,0.));
#7476=DIRECTION('',(-1.,0.,0.));
#7477=DIRECTION('',(0.,0.,1.));
#7478=DIRECTION('',(-1.,0.,0.));
#7479=DIRECTION('',(0.,0.,1.));
#7480=DIRECTION('center_axis',(1.,0.,0.));
#7481=DIRECTION('ref_axis',(0.,1.,0.));
#7482=DIRECTION('',(0.,1.,0.));
#7483=DIRECTION('',(0.,1.,0.));
#7484=DIRECTION('',(0.,0.,1.));
#7485=DIRECTION('center_axis',(0.,-1.,0.));
#7486=DIRECTION('ref_axis',(1.,0.,0.));
#7487=DIRECTION('',(1.,0.,0.));
#7488=DIRECTION('',(1.,0.,0.));
#7489=DIRECTION('',(0.,0.,1.));
#7490=DIRECTION('center_axis',(-1.,0.,0.));
#7491=DIRECTION('ref_axis',(0.,-1.,0.));
#7492=DIRECTION('',(0.,-1.,0.));
#7493=DIRECTION('',(0.,-1.,0.));
#7494=DIRECTION('center_axis',(0.,0.,1.));
#7495=DIRECTION('ref_axis',(1.,0.,0.));
#7496=DIRECTION('center_axis',(0.,0.,1.));
#7497=DIRECTION('ref_axis',(1.,0.,0.));
#7498=DIRECTION('axis',(0.,0.,1.));
#7499=DIRECTION('refdir',(1.,0.,0.));
#7500=DIRECTION('center_axis',(0.,1.,0.));
#7501=DIRECTION('ref_axis',(-1.,0.,0.));
#7502=DIRECTION('',(-1.,0.,0.));
#7503=DIRECTION('',(0.,0.,1.));
#7504=DIRECTION('',(-1.,0.,0.));
#7505=DIRECTION('',(0.,0.,1.));
#7506=DIRECTION('center_axis',(1.,0.,0.));
#7507=DIRECTION('ref_axis',(0.,1.,0.));
#7508=DIRECTION('',(0.,1.,0.));
#7509=DIRECTION('',(0.,1.,0.));
#7510=DIRECTION('',(0.,0.,1.));
#7511=DIRECTION('center_axis',(0.,-1.,0.));
#7512=DIRECTION('ref_axis',(1.,0.,0.));
#7513=DIRECTION('',(1.,0.,0.));
#7514=DIRECTION('',(1.,0.,0.));
#7515=DIRECTION('',(0.,0.,1.));
#7516=DIRECTION('center_axis',(-1.,0.,0.));
#7517=DIRECTION('ref_axis',(0.,-1.,0.));
#7518=DIRECTION('',(0.,-1.,0.));
#7519=DIRECTION('',(0.,-1.,0.));
#7520=DIRECTION('center_axis',(0.,0.,1.));
#7521=DIRECTION('ref_axis',(1.,0.,0.));
#7522=DIRECTION('center_axis',(0.,0.,1.));
#7523=DIRECTION('ref_axis',(1.,0.,0.));
#7524=DIRECTION('axis',(0.,0.,1.));
#7525=DIRECTION('refdir',(1.,0.,0.));
#7526=DIRECTION('center_axis',(0.,1.,0.));
#7527=DIRECTION('ref_axis',(-1.,0.,0.));
#7528=DIRECTION('',(-1.,0.,0.));
#7529=DIRECTION('',(0.,0.,1.));
#7530=DIRECTION('',(-1.,0.,0.));
#7531=DIRECTION('',(0.,0.,1.));
#7532=DIRECTION('center_axis',(1.,0.,0.));
#7533=DIRECTION('ref_axis',(0.,1.,0.));
#7534=DIRECTION('',(0.,1.,0.));
#7535=DIRECTION('',(0.,1.,0.));
#7536=DIRECTION('',(0.,0.,1.));
#7537=DIRECTION('center_axis',(0.,-1.,0.));
#7538=DIRECTION('ref_axis',(1.,0.,0.));
#7539=DIRECTION('',(1.,0.,0.));
#7540=DIRECTION('',(1.,0.,0.));
#7541=DIRECTION('',(0.,0.,1.));
#7542=DIRECTION('center_axis',(-1.,0.,0.));
#7543=DIRECTION('ref_axis',(0.,-1.,0.));
#7544=DIRECTION('',(0.,-1.,0.));
#7545=DIRECTION('',(0.,-1.,0.));
#7546=DIRECTION('center_axis',(0.,0.,1.));
#7547=DIRECTION('ref_axis',(1.,0.,0.));
#7548=DIRECTION('center_axis',(0.,0.,1.));
#7549=DIRECTION('ref_axis',(1.,0.,0.));
#7550=DIRECTION('axis',(0.,0.,1.));
#7551=DIRECTION('refdir',(1.,0.,0.));
#7552=DIRECTION('center_axis',(0.,0.,1.));
#7553=DIRECTION('ref_axis',(1.,0.,0.));
#7554=DIRECTION('center_axis',(0.,0.,1.));
#7555=DIRECTION('ref_axis',(1.,0.,0.));
#7556=DIRECTION('',(0.,0.,1.));
#7557=DIRECTION('center_axis',(0.,0.,-1.));
#7558=DIRECTION('ref_axis',(1.,0.,0.));
#7559=DIRECTION('center_axis',(0.,0.,1.));
#7560=DIRECTION('ref_axis',(1.,0.,0.));
#7561=DIRECTION('center_axis',(0.,0.,1.));
#7562=DIRECTION('ref_axis',(1.,0.,0.));
#7563=DIRECTION('',(0.,0.,1.));
#7564=DIRECTION('center_axis',(0.,0.,-1.));
#7565=DIRECTION('ref_axis',(1.,0.,0.));
#7566=DIRECTION('center_axis',(0.,0.,1.));
#7567=DIRECTION('ref_axis',(1.,0.,0.));
#7568=DIRECTION('center_axis',(0.,0.,1.));
#7569=DIRECTION('ref_axis',(1.,0.,0.));
#7570=DIRECTION('',(0.,0.,1.));
#7571=DIRECTION('center_axis',(0.,0.,-1.));
#7572=DIRECTION('ref_axis',(1.,0.,0.));
#7573=DIRECTION('center_axis',(0.,0.,1.));
#7574=DIRECTION('ref_axis',(1.,0.,0.));
#7575=DIRECTION('center_axis',(0.,0.,1.));
#7576=DIRECTION('ref_axis',(1.,0.,0.));
#7577=DIRECTION('center_axis',(0.,0.,1.));
#7578=DIRECTION('ref_axis',(1.,0.,0.));
#7579=DIRECTION('center_axis',(0.,0.,1.));
#7580=DIRECTION('ref_axis',(1.,0.,0.));
#7581=DIRECTION('',(0.,0.,-1.));
#7582=DIRECTION('center_axis',(0.,0.,-1.));
#7583=DIRECTION('ref_axis',(1.,0.,0.));
#7584=DIRECTION('center_axis',(0.,0.,1.));
#7585=DIRECTION('ref_axis',(1.,0.,0.));
#7586=DIRECTION('center_axis',(0.,0.,1.));
#7587=DIRECTION('ref_axis',(1.,0.,0.));
#7588=DIRECTION('',(0.,0.,-1.));
#7589=DIRECTION('center_axis',(0.,0.,1.));
#7590=DIRECTION('ref_axis',(1.,0.,0.));
#7591=DIRECTION('center_axis',(0.,0.,1.));
#7592=DIRECTION('ref_axis',(1.,0.,0.));
#7593=DIRECTION('center_axis',(0.,0.,1.));
#7594=DIRECTION('ref_axis',(1.,0.,0.));
#7595=DIRECTION('center_axis',(0.,0.,1.));
#7596=DIRECTION('ref_axis',(1.,0.,0.));
#7597=DIRECTION('center_axis',(0.,0.,1.));
#7598=DIRECTION('ref_axis',(1.,0.,0.));
#7599=DIRECTION('',(0.,0.,-1.));
#7600=DIRECTION('center_axis',(0.,0.,1.));
#7601=DIRECTION('ref_axis',(1.,0.,0.));
#7602=DIRECTION('center_axis',(0.,0.,1.));
#7603=DIRECTION('ref_axis',(1.,0.,0.));
#7604=DIRECTION('center_axis',(0.,0.,1.));
#7605=DIRECTION('ref_axis',(1.,0.,0.));
#7606=DIRECTION('',(0.,0.,-1.));
#7607=DIRECTION('center_axis',(0.,0.,1.));
#7608=DIRECTION('ref_axis',(1.,0.,0.));
#7609=DIRECTION('center_axis',(0.,0.,1.));
#7610=DIRECTION('ref_axis',(1.,0.,0.));
#7611=DIRECTION('axis',(0.,0.,1.));
#7612=DIRECTION('refdir',(1.,0.,0.));
#7613=DIRECTION('center_axis',(1.,0.,0.));
#7614=DIRECTION('ref_axis',(0.,0.,-1.));
#7615=DIRECTION('',(0.,0.,1.));
#7616=DIRECTION('center_axis',(1.,0.,0.));
#7617=DIRECTION('ref_axis',(0.,0.,-1.));
#7618=DIRECTION('center_axis',(1.,0.,0.));
#7619=DIRECTION('ref_axis',(0.,0.,-1.));
#7620=DIRECTION('center_axis',(1.,0.,0.));
#7621=DIRECTION('ref_axis',(0.,0.,-1.));
#7622=DIRECTION('',(1.,0.,0.));
#7623=DIRECTION('center_axis',(1.,0.,0.));
#7624=DIRECTION('ref_axis',(0.,0.,-1.));
#7625=DIRECTION('',(0.,0.,-1.));
#7626=DIRECTION('center_axis',(0.,0.,1.));
#7627=DIRECTION('ref_axis',(1.,0.,0.));
#7628=DIRECTION('center_axis',(0.,0.,-1.));
#7629=DIRECTION('ref_axis',(1.,0.,0.));
#7630=DIRECTION('',(0.,0.,-1.));
#7631=DIRECTION('center_axis',(0.,0.,-1.));
#7632=DIRECTION('ref_axis',(1.,0.,0.));
#7633=DIRECTION('center_axis',(0.,0.,1.));
#7634=DIRECTION('ref_axis',(1.,0.,0.));
#7635=DIRECTION('center_axis',(0.,0.,1.));
#7636=DIRECTION('ref_axis',(1.,0.,0.));
#7637=DIRECTION('',(0.,0.,-1.));
#7638=DIRECTION('center_axis',(0.,0.,1.));
#7639=DIRECTION('ref_axis',(1.,0.,0.));
#7640=DIRECTION('center_axis',(0.,0.,1.));
#7641=DIRECTION('ref_axis',(1.,0.,0.));
#7642=DIRECTION('center_axis',(0.,0.,1.));
#7643=DIRECTION('ref_axis',(1.,0.,0.));
#7644=DIRECTION('axis',(0.,0.,1.));
#7645=DIRECTION('refdir',(1.,0.,0.));
#7646=DIRECTION('center_axis',(0.,0.,1.));
#7647=DIRECTION('ref_axis',(1.,0.,0.));
#7648=DIRECTION('center_axis',(0.,0.,1.));
#7649=DIRECTION('ref_axis',(1.,0.,0.));
#7650=DIRECTION('',(0.,0.,1.));
#7651=DIRECTION('center_axis',(0.,0.,1.));
#7652=DIRECTION('ref_axis',(1.,0.,0.));
#7653=DIRECTION('center_axis',(0.,0.,1.));
#7654=DIRECTION('ref_axis',(1.,0.,0.));
#7655=DIRECTION('center_axis',(0.,1.,0.));
#7656=DIRECTION('ref_axis',(1.,0.,0.));
#7657=DIRECTION('',(0.,1.,0.));
#7658=DIRECTION('center_axis',(0.,0.,1.));
#7659=DIRECTION('ref_axis',(1.,0.,0.));
#7660=DIRECTION('center_axis',(0.,0.,1.));
#7661=DIRECTION('ref_axis',(1.,0.,0.));
#7662=DIRECTION('',(0.,0.,-1.));
#7663=DIRECTION('center_axis',(0.,0.,1.));
#7664=DIRECTION('ref_axis',(1.,0.,0.));
#7665=DIRECTION('center_axis',(0.,0.,1.));
#7666=DIRECTION('ref_axis',(1.,0.,0.));
#7667=DIRECTION('center_axis',(0.,0.,1.));
#7668=DIRECTION('ref_axis',(1.,0.,0.));
#7669=DIRECTION('axis',(0.,0.,1.));
#7670=DIRECTION('refdir',(1.,0.,0.));
#7671=DIRECTION('center_axis',(1.,0.,0.));
#7672=DIRECTION('ref_axis',(0.,0.,-1.));
#7673=DIRECTION('center_axis',(1.,0.,0.));
#7674=DIRECTION('ref_axis',(0.,0.,-1.));
#7675=DIRECTION('',(-1.,0.,0.));
#7676=DIRECTION('center_axis',(-0.707106781186545,-0.70710678118655,0.));
#7677=DIRECTION('ref_axis',(-0.70710678118655,0.707106781186545,0.));
#7678=DIRECTION('center_axis',(1.,0.,0.));
#7679=DIRECTION('ref_axis',(0.,0.,-1.));
#7680=DIRECTION('center_axis',(1.,0.,0.));
#7681=DIRECTION('ref_axis',(0.,0.,-1.));
#7682=DIRECTION('center_axis',(1.,0.,0.));
#7683=DIRECTION('ref_axis',(0.,0.,-1.));
#7684=DIRECTION('',(0.,0.,-1.));
#7685=DIRECTION('center_axis',(0.,1.,0.));
#7686=DIRECTION('ref_axis',(1.,0.,0.));
#7687=DIRECTION('center_axis',(0.,1.,0.));
#7688=DIRECTION('ref_axis',(1.,0.,0.));
#7689=DIRECTION('center_axis',(0.,1.,0.));
#7690=DIRECTION('ref_axis',(1.,0.,0.));
#7691=DIRECTION('center_axis',(0.,1.,0.));
#7692=DIRECTION('ref_axis',(1.,0.,0.));
#7693=DIRECTION('center_axis',(0.,1.,0.));
#7694=DIRECTION('ref_axis',(1.,0.,0.));
#7695=DIRECTION('',(0.,-1.,0.));
#7696=DIRECTION('center_axis',(0.,1.,0.));
#7697=DIRECTION('ref_axis',(1.,0.,0.));
#7698=DIRECTION('',(-0.999998524452206,0.,0.00171787467842657));
#7699=DIRECTION('center_axis',(0.000135869566583555,0.996867347600064,0.0790915471354176));
#7700=DIRECTION('ref_axis',(-0.997148648532913,-0.00583337009538651,0.0752365903155829));
#7701=DIRECTION('center_axis',(0.000135869566583555,0.996867347600064,0.0790915471354176));
#7702=DIRECTION('ref_axis',(-0.997148648532913,-0.00583337009538652,0.0752365903155829));
#7703=DIRECTION('center_axis',(-0.000135869608553456,0.996867347637577,
0.0790915466625346));
#7704=DIRECTION('ref_axis',(1.07799070862851E-5,-0.0790915459279024,0.996867356896858));
#7705=DIRECTION('center_axis',(-0.000135869608553456,0.996867347637577,
0.0790915466625346));
#7706=DIRECTION('ref_axis',(1.07799070862851E-5,-0.0790915459279024,0.996867356896858));
#7707=DIRECTION('center_axis',(0.,1.,0.));
#7708=DIRECTION('ref_axis',(1.,0.,0.));
#7709=DIRECTION('center_axis',(0.,1.,0.));
#7710=DIRECTION('ref_axis',(1.,0.,0.));
#7711=DIRECTION('',(0.,-1.,0.));
#7712=DIRECTION('center_axis',(0.,1.,0.));
#7713=DIRECTION('ref_axis',(1.,0.,0.));
#7714=DIRECTION('center_axis',(0.,1.,0.));
#7715=DIRECTION('ref_axis',(1.,0.,0.));
#7716=DIRECTION('',(-0.999998524451277,0.,-0.0017178752193449));
#7717=DIRECTION('center_axis',(0.,1.,0.));
#7718=DIRECTION('ref_axis',(1.,0.,0.));
#7719=DIRECTION('center_axis',(-0.000135869608553456,0.996867347637577,
0.0790915466625346));
#7720=DIRECTION('ref_axis',(1.07799070862851E-5,-0.0790915459279024,0.996867356896858));
#7721=DIRECTION('axis',(0.,0.,1.));
#7722=DIRECTION('refdir',(1.,0.,0.));
#7723=DIRECTION('center_axis',(0.,0.,1.));
#7724=DIRECTION('ref_axis',(1.,0.,0.));
#7725=DIRECTION('center_axis',(0.,0.,1.));
#7726=DIRECTION('ref_axis',(1.,0.,0.));
#7727=DIRECTION('',(0.,0.,1.));
#7728=DIRECTION('center_axis',(0.,0.,1.));
#7729=DIRECTION('ref_axis',(1.,0.,0.));
#7730=DIRECTION('center_axis',(0.,0.,1.));
#7731=DIRECTION('ref_axis',(1.,0.,0.));
#7732=DIRECTION('center_axis',(0.,1.,0.));
#7733=DIRECTION('ref_axis',(1.,0.,0.));
#7734=DIRECTION('center_axis',(0.,1.,0.));
#7735=DIRECTION('ref_axis',(1.,0.,0.));
#7736=DIRECTION('',(0.,1.,0.));
#7737=DIRECTION('center_axis',(0.,-1.,0.));
#7738=DIRECTION('ref_axis',(1.,0.,0.));
#7739=DIRECTION('center_axis',(0.,1.,0.));
#7740=DIRECTION('ref_axis',(-1.,0.,0.));
#7741=DIRECTION('',(-1.,0.,0.));
#7742=DIRECTION('',(0.,0.,1.));
#7743=DIRECTION('',(-1.,0.,0.));
#7744=DIRECTION('',(0.,0.,1.));
#7745=DIRECTION('center_axis',(1.,0.,0.));
#7746=DIRECTION('ref_axis',(0.,1.,0.));
#7747=DIRECTION('',(0.,1.,0.));
#7748=DIRECTION('',(0.,1.,0.));
#7749=DIRECTION('',(0.,0.,1.));
#7750=DIRECTION('center_axis',(0.,-1.,0.));
#7751=DIRECTION('ref_axis',(1.,0.,0.));
#7752=DIRECTION('',(1.,0.,0.));
#7753=DIRECTION('',(1.,0.,0.));
#7754=DIRECTION('',(0.,0.,1.));
#7755=DIRECTION('center_axis',(-1.,0.,0.));
#7756=DIRECTION('ref_axis',(0.,-1.,0.));
#7757=DIRECTION('',(0.,-1.,0.));
#7758=DIRECTION('',(0.,-1.,0.));
#7759=DIRECTION('center_axis',(0.,0.,1.));
#7760=DIRECTION('ref_axis',(1.,0.,0.));
#7761=DIRECTION('center_axis',(0.,0.,1.));
#7762=DIRECTION('ref_axis',(1.,0.,0.));
#7763=DIRECTION('axis',(0.,0.,1.));
#7764=DIRECTION('refdir',(1.,0.,0.));
#7765=DIRECTION('center_axis',(0.,1.,0.));
#7766=DIRECTION('ref_axis',(1.,0.,0.));
#7767=DIRECTION('center_axis',(0.,1.,0.));
#7768=DIRECTION('ref_axis',(1.,0.,0.));
#7769=DIRECTION('',(0.707106781186548,-0.707106781186547,-8.65956056235494E-17));
#7770=DIRECTION('center_axis',(0.,-1.,0.));
#7771=DIRECTION('ref_axis',(1.,0.,0.));
#7772=DIRECTION('center_axis',(0.,1.,0.));
#7773=DIRECTION('ref_axis',(1.,0.,0.));
#7774=DIRECTION('',(0.,-1.,0.));
#7775=DIRECTION('center_axis',(0.,-1.,0.));
#7776=DIRECTION('ref_axis',(1.,0.,0.));
#7777=DIRECTION('center_axis',(0.,1.,0.));
#7778=DIRECTION('ref_axis',(1.,0.,0.));
#7779=DIRECTION('center_axis',(0.,1.,0.));
#7780=DIRECTION('ref_axis',(1.,0.,0.));
#7781=DIRECTION('center_axis',(0.,1.,0.));
#7782=DIRECTION('ref_axis',(1.,0.,0.));
#7783=DIRECTION('',(0.,-1.,0.));
#7784=DIRECTION('center_axis',(0.,1.,0.));
#7785=DIRECTION('ref_axis',(1.,0.,0.));
#7786=DIRECTION('center_axis',(0.,1.,0.));
#7787=DIRECTION('ref_axis',(1.,0.,0.));
#7788=DIRECTION('axis',(0.,0.,1.));
#7789=DIRECTION('refdir',(1.,0.,0.));
#7790=DIRECTION('center_axis',(0.,1.,0.));
#7791=DIRECTION('ref_axis',(0.,0.,1.));
#7792=DIRECTION('center_axis',(0.,-1.,0.));
#7793=DIRECTION('ref_axis',(1.,0.,0.));
#7794=DIRECTION('center_axis',(0.,-1.,0.));
#7795=DIRECTION('ref_axis',(1.,0.,0.));
#7796=DIRECTION('center_axis',(0.,-1.,0.));
#7797=DIRECTION('ref_axis',(1.,0.,0.));
#7798=DIRECTION('',(0.707106781186548,0.707106781186547,8.65956056235493E-17));
#7799=DIRECTION('center_axis',(0.,-1.,0.));
#7800=DIRECTION('ref_axis',(1.,0.,0.));
#7801=DIRECTION('center_axis',(0.,-1.,0.));
#7802=DIRECTION('ref_axis',(1.,0.,0.));
#7803=DIRECTION('',(0.,1.,0.));
#7804=DIRECTION('center_axis',(0.,1.,0.));
#7805=DIRECTION('ref_axis',(1.,0.,0.));
#7806=DIRECTION('center_axis',(0.,-1.,0.));
#7807=DIRECTION('ref_axis',(1.,0.,0.));
#7808=DIRECTION('',(-0.707106781186547,0.707106781186548,-8.65956056235493E-17));
#7809=DIRECTION('center_axis',(0.,-1.,0.));
#7810=DIRECTION('ref_axis',(0.,0.,-1.));
#7811=DIRECTION('center_axis',(0.,-1.,0.));
#7812=DIRECTION('ref_axis',(1.,0.,0.));
#7813=DIRECTION('center_axis',(0.,1.,0.));
#7814=DIRECTION('ref_axis',(1.,0.,0.));
#7815=DIRECTION('center_axis',(0.,1.,0.));
#7816=DIRECTION('ref_axis',(1.,0.,0.));
#7817=DIRECTION('',(-0.447213595499958,0.894427190999916,-5.47678698264203E-17));
#7818=DIRECTION('center_axis',(0.,-1.,0.));
#7819=DIRECTION('ref_axis',(1.,0.,0.));
#7820=DIRECTION('center_axis',(0.,1.,0.));
#7821=DIRECTION('ref_axis',(1.,0.,0.));
#7822=DIRECTION('',(0.,1.,0.));
#7823=DIRECTION('center_axis',(0.,1.,0.));
#7824=DIRECTION('ref_axis',(1.,0.,0.));
#7825=DIRECTION('center_axis',(0.,-1.,0.));
#7826=DIRECTION('ref_axis',(1.,0.,0.));
#7827=DIRECTION('',(-0.707106781186547,0.707106781186548,-8.65956056235493E-17));
#7828=DIRECTION('center_axis',(0.,-1.,0.));
#7829=DIRECTION('ref_axis',(0.,0.,-1.));
#7830=DIRECTION('center_axis',(0.866025403784439,0.,-0.5));
#7831=DIRECTION('ref_axis',(0.5,0.,0.866025403784439));
#7832=DIRECTION('',(-0.5,0.,-0.866025403784439));
#7833=DIRECTION('',(0.,-1.,0.));
#7834=DIRECTION('',(0.5,0.,0.866025403784439));
#7835=DIRECTION('',(0.,-1.,0.));
#7836=DIRECTION('center_axis',(1.20185167898973E-16,0.,-1.));
#7837=DIRECTION('ref_axis',(1.,0.,1.20185167898973E-16));
#7838=DIRECTION('',(-1.,0.,-1.20185167898973E-16));
#7839=DIRECTION('',(0.,-1.,0.));
#7840=DIRECTION('',(1.,0.,1.20185167898973E-16));
#7841=DIRECTION('center_axis',(-0.866025403784439,0.,-0.5));
#7842=DIRECTION('ref_axis',(0.5,0.,-0.866025403784439));
#7843=DIRECTION('',(-0.5,0.,0.866025403784439));
#7844=DIRECTION('',(0.,-1.,0.));
#7845=DIRECTION('',(0.5,0.,-0.866025403784439));
#7846=DIRECTION('center_axis',(-0.866025403784439,0.,0.5));
#7847=DIRECTION('ref_axis',(-0.5,0.,-0.866025403784439));
#7848=DIRECTION('',(0.5,0.,0.866025403784439));
#7849=DIRECTION('',(0.,-1.,0.));
#7850=DIRECTION('',(-0.5,0.,-0.866025403784439));
#7851=DIRECTION('center_axis',(-2.40370335797945E-16,0.,1.));
#7852=DIRECTION('ref_axis',(-1.,0.,-2.40370335797945E-16));
#7853=DIRECTION('',(1.,0.,2.40370335797945E-16));
#7854=DIRECTION('',(0.,-1.,0.));
#7855=DIRECTION('',(-1.,0.,-2.40370335797945E-16));
#7856=DIRECTION('center_axis',(0.866025403784439,0.,0.5));
#7857=DIRECTION('ref_axis',(-0.5,0.,0.866025403784439));
#7858=DIRECTION('',(0.5,0.,-0.866025403784439));
#7859=DIRECTION('',(-0.5,0.,0.866025403784439));
#7860=DIRECTION('center_axis',(0.,1.,0.));
#7861=DIRECTION('ref_axis',(1.,0.,0.));
#7862=DIRECTION('center_axis',(0.,-1.,0.));
#7863=DIRECTION('ref_axis',(0.,0.,-1.));
#7864=DIRECTION('axis',(0.,0.,1.));
#7865=DIRECTION('refdir',(1.,0.,0.));
#7866=DIRECTION('center_axis',(0.,1.,0.));
#7867=DIRECTION('ref_axis',(1.,0.,0.));
#7868=DIRECTION('',(0.866025403784439,-0.5,1.06057523872491E-16));
#7869=DIRECTION('center_axis',(0.,-1.,0.));
#7870=DIRECTION('ref_axis',(1.,0.,0.));
#7871=DIRECTION('center_axis',(0.,-1.,0.));
#7872=DIRECTION('ref_axis',(1.,0.,0.));
#7873=DIRECTION('center_axis',(0.,1.,0.));
#7874=DIRECTION('ref_axis',(1.,0.,0.));
#7875=DIRECTION('',(-0.866025403784439,-0.5,-1.06057523872491E-16));
#7876=DIRECTION('center_axis',(1.20185167898973E-16,0.,-1.));
#7877=DIRECTION('ref_axis',(-1.,0.,-1.20185167898973E-16));
#7878=DIRECTION('',(0.,1.,0.));
#7879=DIRECTION('',(0.,1.,0.));
#7880=DIRECTION('center_axis',(-0.866025403784439,0.,-0.5));
#7881=DIRECTION('ref_axis',(-0.5,0.,0.866025403784439));
#7882=DIRECTION('',(0.,1.,0.));
#7883=DIRECTION('center_axis',(-0.866025403784439,0.,0.5));
#7884=DIRECTION('ref_axis',(0.5,0.,0.866025403784439));
#7885=DIRECTION('',(0.,1.,0.));
#7886=DIRECTION('center_axis',(0.,1.,0.));
#7887=DIRECTION('ref_axis',(1.,0.,0.));
#7888=DIRECTION('center_axis',(0.,1.,0.));
#7889=DIRECTION('ref_axis',(1.,0.,0.));
#7890=DIRECTION('',(0.,-1.,0.));
#7891=DIRECTION('center_axis',(0.,1.,0.));
#7892=DIRECTION('ref_axis',(1.,0.,0.));
#7893=DIRECTION('center_axis',(-2.40370335797945E-16,0.,1.));
#7894=DIRECTION('ref_axis',(1.,0.,2.40370335797945E-16));
#7895=DIRECTION('',(0.,1.,0.));
#7896=DIRECTION('center_axis',(0.866025403784439,0.,-0.5));
#7897=DIRECTION('ref_axis',(-0.5,0.,-0.866025403784439));
#7898=DIRECTION('',(0.,1.,0.));
#7899=DIRECTION('center_axis',(0.866025403784439,0.,0.5));
#7900=DIRECTION('ref_axis',(0.5,0.,-0.866025403784439));
#7901=DIRECTION('center_axis',(0.,1.,0.));
#7902=DIRECTION('ref_axis',(1.,0.,0.));
#7903=DIRECTION('center_axis',(0.,1.,0.));
#7904=DIRECTION('ref_axis',(1.,0.,0.));
#7905=DIRECTION('axis',(0.,0.,1.));
#7906=DIRECTION('refdir',(1.,0.,0.));
#7907=DIRECTION('center_axis',(0.,1.,0.));
#7908=DIRECTION('ref_axis',(0.,0.,1.));
#7909=DIRECTION('center_axis',(0.,-1.,0.));
#7910=DIRECTION('ref_axis',(1.,0.,0.));
#7911=DIRECTION('center_axis',(0.,-1.,0.));
#7912=DIRECTION('ref_axis',(1.,0.,0.));
#7913=DIRECTION('center_axis',(0.,-1.,0.));
#7914=DIRECTION('ref_axis',(1.,0.,0.));
#7915=DIRECTION('',(0.707106781186547,0.707106781186548,8.65956056235493E-17));
#7916=DIRECTION('center_axis',(0.,-1.,0.));
#7917=DIRECTION('ref_axis',(1.,0.,0.));
#7918=DIRECTION('center_axis',(0.,-1.,0.));
#7919=DIRECTION('ref_axis',(1.,0.,0.));
#7920=DIRECTION('',(0.,1.,0.));
#7921=DIRECTION('center_axis',(0.,1.,0.));
#7922=DIRECTION('ref_axis',(1.,0.,0.));
#7923=DIRECTION('center_axis',(0.,-1.,0.));
#7924=DIRECTION('ref_axis',(1.,0.,0.));
#7925=DIRECTION('',(-0.707106781186547,0.707106781186548,-8.65956056235493E-17));
#7926=DIRECTION('center_axis',(0.,-1.,0.));
#7927=DIRECTION('ref_axis',(0.,0.,-1.));
#7928=DIRECTION('center_axis',(0.,-1.,0.));
#7929=DIRECTION('ref_axis',(1.,0.,0.));
#7930=DIRECTION('center_axis',(0.,1.,0.));
#7931=DIRECTION('ref_axis',(1.,0.,0.));
#7932=DIRECTION('center_axis',(0.,1.,0.));
#7933=DIRECTION('ref_axis',(1.,0.,0.));
#7934=DIRECTION('',(-0.447213595499958,0.894427190999916,-5.47678698264203E-17));
#7935=DIRECTION('center_axis',(0.,-1.,0.));
#7936=DIRECTION('ref_axis',(1.,0.,0.));
#7937=DIRECTION('center_axis',(0.,1.,0.));
#7938=DIRECTION('ref_axis',(1.,0.,0.));
#7939=DIRECTION('',(0.,1.,0.));
#7940=DIRECTION('center_axis',(0.,1.,0.));
#7941=DIRECTION('ref_axis',(1.,0.,0.));
#7942=DIRECTION('center_axis',(0.,-1.,0.));
#7943=DIRECTION('ref_axis',(1.,0.,0.));
#7944=DIRECTION('',(-0.707106781186547,0.707106781186548,-8.65956056235493E-17));
#7945=DIRECTION('center_axis',(0.,-1.,0.));
#7946=DIRECTION('ref_axis',(0.,0.,-1.));
#7947=DIRECTION('center_axis',(0.866025403784439,0.,-0.5));
#7948=DIRECTION('ref_axis',(0.5,0.,0.866025403784439));
#7949=DIRECTION('',(-0.5,0.,-0.866025403784439));
#7950=DIRECTION('',(0.,-1.,0.));
#7951=DIRECTION('',(0.5,0.,0.866025403784439));
#7952=DIRECTION('',(0.,-1.,0.));
#7953=DIRECTION('center_axis',(1.60246890531964E-16,0.,-1.));
#7954=DIRECTION('ref_axis',(1.,0.,1.60246890531964E-16));
#7955=DIRECTION('',(-1.,0.,-1.60246890531964E-16));
#7956=DIRECTION('',(0.,-1.,0.));
#7957=DIRECTION('',(1.,0.,1.60246890531964E-16));
#7958=DIRECTION('center_axis',(-0.866025403784439,0.,-0.5));
#7959=DIRECTION('ref_axis',(0.5,0.,-0.866025403784439));
#7960=DIRECTION('',(-0.5,0.,0.866025403784439));
#7961=DIRECTION('',(0.,-1.,0.));
#7962=DIRECTION('',(0.5,0.,-0.866025403784439));
#7963=DIRECTION('center_axis',(-0.866025403784439,0.,0.5));
#7964=DIRECTION('ref_axis',(-0.5,0.,-0.866025403784439));
#7965=DIRECTION('',(0.5,0.,0.866025403784439));
#7966=DIRECTION('',(0.,-1.,0.));
#7967=DIRECTION('',(-0.5,0.,-0.866025403784439));
#7968=DIRECTION('center_axis',(-1.60246890531964E-16,0.,1.));
#7969=DIRECTION('ref_axis',(-1.,0.,-1.60246890531964E-16));
#7970=DIRECTION('',(1.,0.,1.60246890531964E-16));
#7971=DIRECTION('',(0.,-1.,0.));
#7972=DIRECTION('',(-1.,0.,-1.60246890531964E-16));
#7973=DIRECTION('center_axis',(0.866025403784439,0.,0.5));
#7974=DIRECTION('ref_axis',(-0.5,0.,0.866025403784439));
#7975=DIRECTION('',(0.5,0.,-0.866025403784439));
#7976=DIRECTION('',(-0.5,0.,0.866025403784439));
#7977=DIRECTION('center_axis',(0.,1.,0.));
#7978=DIRECTION('ref_axis',(1.,0.,0.));
#7979=DIRECTION('center_axis',(0.,-1.,0.));
#7980=DIRECTION('ref_axis',(0.,0.,-1.));
#7981=DIRECTION('axis',(0.,0.,1.));
#7982=DIRECTION('refdir',(1.,0.,0.));
#7983=DIRECTION('axis',(0.,0.,1.));
#7984=DIRECTION('refdir',(1.,0.,0.));
#7985=DIRECTION('center_axis',(0.,0.,1.));
#7986=DIRECTION('ref_axis',(1.,0.,0.));
#7987=DIRECTION('center_axis',(0.,0.,1.));
#7988=DIRECTION('ref_axis',(1.,0.,0.));
#7989=DIRECTION('',(0.,0.,1.));
#7990=DIRECTION('center_axis',(0.,0.,-1.));
#7991=DIRECTION('ref_axis',(1.,0.,0.));
#7992=DIRECTION('center_axis',(0.,0.,1.));
#7993=DIRECTION('ref_axis',(1.,0.,0.));
#7994=DIRECTION('center_axis',(0.,0.,1.));
#7995=DIRECTION('ref_axis',(1.,0.,0.));
#7996=DIRECTION('',(0.,0.,1.));
#7997=DIRECTION('center_axis',(0.,0.,-1.));
#7998=DIRECTION('ref_axis',(1.,0.,0.));
#7999=DIRECTION('center_axis',(0.,0.,1.));
#8000=DIRECTION('ref_axis',(1.,0.,0.));
#8001=DIRECTION('center_axis',(0.,0.,1.));
#8002=DIRECTION('ref_axis',(1.,0.,0.));
#8003=DIRECTION('',(0.,0.,1.));
#8004=DIRECTION('center_axis',(0.,0.,-1.));
#8005=DIRECTION('ref_axis',(1.,0.,0.));
#8006=DIRECTION('center_axis',(0.,0.,1.));
#8007=DIRECTION('ref_axis',(1.,0.,0.));
#8008=DIRECTION('center_axis',(0.,0.,1.));
#8009=DIRECTION('ref_axis',(1.,0.,0.));
#8010=DIRECTION('',(0.,0.,1.));
#8011=DIRECTION('center_axis',(0.,0.,-1.));
#8012=DIRECTION('ref_axis',(1.,0.,0.));
#8013=DIRECTION('center_axis',(0.,0.,1.));
#8014=DIRECTION('ref_axis',(1.,0.,0.));
#8015=DIRECTION('center_axis',(0.,0.,1.));
#8016=DIRECTION('ref_axis',(1.,0.,0.));
#8017=DIRECTION('',(0.,0.,1.));
#8018=DIRECTION('center_axis',(0.,0.,-1.));
#8019=DIRECTION('ref_axis',(1.,0.,0.));
#8020=DIRECTION('center_axis',(0.,0.,1.));
#8021=DIRECTION('ref_axis',(1.,0.,0.));
#8022=DIRECTION('center_axis',(0.,0.,1.));
#8023=DIRECTION('ref_axis',(1.,0.,0.));
#8024=DIRECTION('',(0.,0.,1.));
#8025=DIRECTION('center_axis',(0.,0.,-1.));
#8026=DIRECTION('ref_axis',(1.,0.,0.));
#8027=DIRECTION('center_axis',(0.,0.,1.));
#8028=DIRECTION('ref_axis',(1.,0.,0.));
#8029=DIRECTION('center_axis',(0.,0.,1.));
#8030=DIRECTION('ref_axis',(1.,0.,0.));
#8031=DIRECTION('',(0.,0.,1.));
#8032=DIRECTION('center_axis',(0.,0.,-1.));
#8033=DIRECTION('ref_axis',(1.,0.,0.));
#8034=DIRECTION('center_axis',(0.,0.,1.));
#8035=DIRECTION('ref_axis',(1.,0.,0.));
#8036=DIRECTION('center_axis',(0.,0.,1.));
#8037=DIRECTION('ref_axis',(1.,0.,0.));
#8038=DIRECTION('',(0.,0.,1.));
#8039=DIRECTION('center_axis',(0.,0.,-1.));
#8040=DIRECTION('ref_axis',(1.,0.,0.));
#8041=DIRECTION('center_axis',(0.,0.,1.));
#8042=DIRECTION('ref_axis',(1.,0.,0.));
#8043=DIRECTION('center_axis',(0.,0.,1.));
#8044=DIRECTION('ref_axis',(1.,0.,0.));
#8045=DIRECTION('',(0.,0.,1.));
#8046=DIRECTION('center_axis',(0.,0.,-1.));
#8047=DIRECTION('ref_axis',(1.,0.,0.));
#8048=DIRECTION('center_axis',(0.,0.,1.));
#8049=DIRECTION('ref_axis',(1.,0.,0.));
#8050=DIRECTION('center_axis',(0.,0.,1.));
#8051=DIRECTION('ref_axis',(1.,0.,0.));
#8052=DIRECTION('',(0.,0.,1.));
#8053=DIRECTION('center_axis',(0.,0.,-1.));
#8054=DIRECTION('ref_axis',(1.,0.,0.));
#8055=DIRECTION('center_axis',(0.,0.,1.));
#8056=DIRECTION('ref_axis',(1.,0.,0.));
#8057=DIRECTION('',(0.,0.,-1.));
#8058=DIRECTION('center_axis',(0.,0.,1.));
#8059=DIRECTION('ref_axis',(1.,0.,0.));
#8060=DIRECTION('',(0.,0.,1.));
#8061=DIRECTION('center_axis',(0.,0.,1.));
#8062=DIRECTION('ref_axis',(1.,0.,0.));
#8063=DIRECTION('center_axis',(0.,1.,0.));
#8064=DIRECTION('ref_axis',(-1.,0.,0.));
#8065=DIRECTION('',(-1.,0.,0.));
#8066=DIRECTION('',(0.,0.,-1.));
#8067=DIRECTION('',(-1.,0.,0.));
#8068=DIRECTION('center_axis',(0.,0.,1.));
#8069=DIRECTION('ref_axis',(1.,0.,0.));
#8070=DIRECTION('',(1.,0.,0.));
#8071=DIRECTION('center_axis',(0.,0.,1.));
#8072=DIRECTION('ref_axis',(1.,0.,0.));
#8073=DIRECTION('center_axis',(0.,-1.,0.));
#8074=DIRECTION('ref_axis',(1.,0.,0.));
#8075=DIRECTION('',(1.,0.,0.));
#8076=DIRECTION('',(0.,0.,1.));
#8077=DIRECTION('center_axis',(0.,0.,1.));
#8078=DIRECTION('ref_axis',(-1.,1.22464679914735E-16,0.));
#8079=DIRECTION('center_axis',(0.,0.,1.));
#8080=DIRECTION('ref_axis',(1.,0.,0.));
#8081=DIRECTION('center_axis',(0.,0.,1.));
#8082=DIRECTION('ref_axis',(1.,0.,0.));
#8083=DIRECTION('axis',(0.,0.,1.));
#8084=DIRECTION('refdir',(1.,0.,0.));
#8085=DIRECTION('center_axis',(0.,0.,1.));
#8086=DIRECTION('ref_axis',(1.,0.,0.));
#8087=DIRECTION('center_axis',(0.,0.,1.));
#8088=DIRECTION('ref_axis',(1.,0.,0.));
#8089=DIRECTION('',(0.,0.,1.));
#8090=DIRECTION('center_axis',(0.,0.,-1.));
#8091=DIRECTION('ref_axis',(1.,0.,0.));
#8092=DIRECTION('center_axis',(0.,0.,1.));
#8093=DIRECTION('ref_axis',(1.,0.,0.));
#8094=DIRECTION('center_axis',(0.,0.,1.));
#8095=DIRECTION('ref_axis',(1.,0.,0.));
#8096=DIRECTION('',(0.,0.,1.));
#8097=DIRECTION('center_axis',(0.,0.,-1.));
#8098=DIRECTION('ref_axis',(1.,0.,0.));
#8099=DIRECTION('center_axis',(0.,0.,1.));
#8100=DIRECTION('ref_axis',(1.,0.,0.));
#8101=DIRECTION('center_axis',(0.,0.,1.));
#8102=DIRECTION('ref_axis',(1.,0.,0.));
#8103=DIRECTION('',(0.,0.,1.));
#8104=DIRECTION('center_axis',(0.,0.,-1.));
#8105=DIRECTION('ref_axis',(1.,0.,0.));
#8106=DIRECTION('center_axis',(0.,0.,1.));
#8107=DIRECTION('ref_axis',(1.,0.,0.));
#8108=DIRECTION('center_axis',(0.,0.,1.));
#8109=DIRECTION('ref_axis',(1.,0.,0.));
#8110=DIRECTION('',(0.,0.,1.));
#8111=DIRECTION('center_axis',(0.,0.,-1.));
#8112=DIRECTION('ref_axis',(1.,0.,0.));
#8113=DIRECTION('center_axis',(0.,0.,1.));
#8114=DIRECTION('ref_axis',(1.,0.,0.));
#8115=DIRECTION('center_axis',(0.,0.,1.));
#8116=DIRECTION('ref_axis',(1.,0.,0.));
#8117=DIRECTION('',(0.,0.,-1.));
#8118=DIRECTION('center_axis',(0.,0.,-1.));
#8119=DIRECTION('ref_axis',(1.,0.,0.));
#8120=DIRECTION('center_axis',(0.,0.,1.));
#8121=DIRECTION('ref_axis',(1.,0.,0.));
#8122=DIRECTION('center_axis',(0.,0.,-1.));
#8123=DIRECTION('ref_axis',(1.,0.,0.));
#8124=DIRECTION('center_axis',(0.,0.,1.));
#8125=DIRECTION('ref_axis',(1.,0.,0.));
#8126=DIRECTION('',(0.,0.,-1.));
#8127=DIRECTION('center_axis',(0.,0.,-1.));
#8128=DIRECTION('ref_axis',(1.,0.,0.));
#8129=DIRECTION('center_axis',(0.,0.,1.));
#8130=DIRECTION('ref_axis',(1.,0.,0.));
#8131=DIRECTION('center_axis',(0.,0.,1.));
#8132=DIRECTION('ref_axis',(1.,0.,0.));
#8133=DIRECTION('',(0.,0.,-1.));
#8134=DIRECTION('center_axis',(0.,0.,1.));
#8135=DIRECTION('ref_axis',(1.,0.,0.));
#8136=DIRECTION('center_axis',(0.,0.,1.));
#8137=DIRECTION('ref_axis',(1.,0.,0.));
#8138=DIRECTION('center_axis',(0.,0.,1.));
#8139=DIRECTION('ref_axis',(1.,0.,0.));
#8140=DIRECTION('axis',(0.,0.,1.));
#8141=DIRECTION('refdir',(1.,0.,0.));
#8142=DIRECTION('center_axis',(0.,0.,1.));
#8143=DIRECTION('ref_axis',(1.,0.,0.));
#8144=DIRECTION('center_axis',(0.,0.,1.));
#8145=DIRECTION('ref_axis',(1.,0.,0.));
#8146=DIRECTION('',(0.,0.,1.));
#8147=DIRECTION('center_axis',(0.,0.,-1.));
#8148=DIRECTION('ref_axis',(1.,0.,0.));
#8149=DIRECTION('center_axis',(0.,0.,1.));
#8150=DIRECTION('ref_axis',(1.,0.,0.));
#8151=DIRECTION('center_axis',(0.,0.,1.));
#8152=DIRECTION('ref_axis',(1.,0.,0.));
#8153=DIRECTION('',(0.,0.,1.));
#8154=DIRECTION('center_axis',(0.,0.,-1.));
#8155=DIRECTION('ref_axis',(1.,0.,0.));
#8156=DIRECTION('center_axis',(0.,0.,1.));
#8157=DIRECTION('ref_axis',(1.,0.,0.));
#8158=DIRECTION('center_axis',(0.,0.,1.));
#8159=DIRECTION('ref_axis',(1.,0.,0.));
#8160=DIRECTION('',(0.,0.,1.));
#8161=DIRECTION('center_axis',(0.,0.,-1.));
#8162=DIRECTION('ref_axis',(1.,0.,0.));
#8163=DIRECTION('center_axis',(0.,0.,1.));
#8164=DIRECTION('ref_axis',(1.,0.,0.));
#8165=DIRECTION('center_axis',(0.,0.,1.));
#8166=DIRECTION('ref_axis',(1.,0.,0.));
#8167=DIRECTION('',(0.,0.,1.));
#8168=DIRECTION('center_axis',(0.,0.,-1.));
#8169=DIRECTION('ref_axis',(1.,0.,0.));
#8170=DIRECTION('center_axis',(0.,0.,1.));
#8171=DIRECTION('ref_axis',(1.,0.,0.));
#8172=DIRECTION('center_axis',(0.,0.,1.));
#8173=DIRECTION('ref_axis',(1.,0.,0.));
#8174=DIRECTION('',(0.,0.,-1.));
#8175=DIRECTION('center_axis',(0.,0.,1.));
#8176=DIRECTION('ref_axis',(1.,0.,0.));
#8177=DIRECTION('center_axis',(0.,0.,1.));
#8178=DIRECTION('ref_axis',(1.,0.,0.));
#8179=DIRECTION('center_axis',(0.,0.,-1.));
#8180=DIRECTION('ref_axis',(1.,0.,0.));
#8181=DIRECTION('center_axis',(0.,0.,1.));
#8182=DIRECTION('ref_axis',(1.,0.,0.));
#8183=DIRECTION('center_axis',(0.,0.,-1.));
#8184=DIRECTION('ref_axis',(1.,0.,0.));
#8185=DIRECTION('',(0.,0.,-1.));
#8186=DIRECTION('center_axis',(0.,0.,1.));
#8187=DIRECTION('ref_axis',(1.,0.,0.));
#8188=DIRECTION('center_axis',(0.,0.,1.));
#8189=DIRECTION('ref_axis',(1.,0.,0.));
#8190=DIRECTION('',(0.,0.,-1.));
#8191=DIRECTION('center_axis',(0.,0.,1.));
#8192=DIRECTION('ref_axis',(1.,0.,0.));
#8193=DIRECTION('center_axis',(0.,0.,1.));
#8194=DIRECTION('ref_axis',(1.,0.,0.));
#8195=DIRECTION('center_axis',(0.,0.,1.));
#8196=DIRECTION('ref_axis',(1.,0.,0.));
#8197=DIRECTION('axis',(0.,0.,1.));
#8198=DIRECTION('refdir',(1.,0.,0.));
#8199=DIRECTION('center_axis',(0.,0.,1.));
#8200=DIRECTION('ref_axis',(1.,0.,0.));
#8201=DIRECTION('center_axis',(0.,0.,1.));
#8202=DIRECTION('ref_axis',(1.,0.,0.));
#8203=DIRECTION('',(0.,0.,1.));
#8204=DIRECTION('center_axis',(0.,0.,-1.));
#8205=DIRECTION('ref_axis',(1.,0.,0.));
#8206=DIRECTION('center_axis',(0.,0.,1.));
#8207=DIRECTION('ref_axis',(1.,0.,0.));
#8208=DIRECTION('center_axis',(0.,0.,1.));
#8209=DIRECTION('ref_axis',(1.,0.,0.));
#8210=DIRECTION('',(0.,0.,1.));
#8211=DIRECTION('center_axis',(0.,0.,-1.));
#8212=DIRECTION('ref_axis',(1.,0.,0.));
#8213=DIRECTION('center_axis',(0.,0.,1.));
#8214=DIRECTION('ref_axis',(1.,0.,0.));
#8215=DIRECTION('center_axis',(0.,0.,1.));
#8216=DIRECTION('ref_axis',(1.,0.,0.));
#8217=DIRECTION('',(0.,0.,1.));
#8218=DIRECTION('center_axis',(0.,0.,-1.));
#8219=DIRECTION('ref_axis',(1.,0.,0.));
#8220=DIRECTION('center_axis',(0.,0.,1.));
#8221=DIRECTION('ref_axis',(1.,0.,0.));
#8222=DIRECTION('center_axis',(0.,0.,1.));
#8223=DIRECTION('ref_axis',(1.,0.,0.));
#8224=DIRECTION('',(0.,0.,1.));
#8225=DIRECTION('center_axis',(0.,0.,-1.));
#8226=DIRECTION('ref_axis',(1.,0.,0.));
#8227=DIRECTION('center_axis',(0.,0.,1.));
#8228=DIRECTION('ref_axis',(1.,0.,0.));
#8229=DIRECTION('center_axis',(0.,0.,1.));
#8230=DIRECTION('ref_axis',(1.,0.,0.));
#8231=DIRECTION('',(0.,0.,-1.));
#8232=DIRECTION('center_axis',(0.,0.,-1.));
#8233=DIRECTION('ref_axis',(1.,0.,0.));
#8234=DIRECTION('center_axis',(0.,0.,1.));
#8235=DIRECTION('ref_axis',(1.,0.,0.));
#8236=DIRECTION('center_axis',(0.,0.,-1.));
#8237=DIRECTION('ref_axis',(1.,0.,0.));
#8238=DIRECTION('center_axis',(0.,0.,1.));
#8239=DIRECTION('ref_axis',(1.,0.,0.));
#8240=DIRECTION('',(0.,0.,-1.));
#8241=DIRECTION('center_axis',(0.,0.,-1.));
#8242=DIRECTION('ref_axis',(1.,0.,0.));
#8243=DIRECTION('center_axis',(0.,0.,1.));
#8244=DIRECTION('ref_axis',(1.,0.,0.));
#8245=DIRECTION('center_axis',(0.,0.,1.));
#8246=DIRECTION('ref_axis',(1.,0.,0.));
#8247=DIRECTION('',(0.,0.,-1.));
#8248=DIRECTION('center_axis',(0.,0.,1.));
#8249=DIRECTION('ref_axis',(1.,0.,0.));
#8250=DIRECTION('center_axis',(0.,0.,1.));
#8251=DIRECTION('ref_axis',(1.,0.,0.));
#8252=DIRECTION('center_axis',(0.,0.,1.));
#8253=DIRECTION('ref_axis',(1.,0.,0.));
#8254=DIRECTION('axis',(0.,0.,1.));
#8255=DIRECTION('refdir',(1.,0.,0.));
#8256=DIRECTION('center_axis',(0.,0.,1.));
#8257=DIRECTION('ref_axis',(1.,0.,0.));
#8258=DIRECTION('center_axis',(0.,0.,1.));
#8259=DIRECTION('ref_axis',(1.,0.,0.));
#8260=DIRECTION('',(0.,0.,1.));
#8261=DIRECTION('center_axis',(0.,0.,-1.));
#8262=DIRECTION('ref_axis',(1.,0.,0.));
#8263=DIRECTION('center_axis',(0.,0.,1.));
#8264=DIRECTION('ref_axis',(1.,0.,0.));
#8265=DIRECTION('center_axis',(0.,0.,1.));
#8266=DIRECTION('ref_axis',(1.,0.,0.));
#8267=DIRECTION('',(0.,0.,1.));
#8268=DIRECTION('center_axis',(0.,0.,-1.));
#8269=DIRECTION('ref_axis',(1.,0.,0.));
#8270=DIRECTION('center_axis',(0.,0.,1.));
#8271=DIRECTION('ref_axis',(1.,0.,0.));
#8272=DIRECTION('center_axis',(0.,0.,1.));
#8273=DIRECTION('ref_axis',(1.,0.,0.));
#8274=DIRECTION('',(0.,0.,1.));
#8275=DIRECTION('center_axis',(0.,0.,-1.));
#8276=DIRECTION('ref_axis',(1.,0.,0.));
#8277=DIRECTION('center_axis',(0.,0.,1.));
#8278=DIRECTION('ref_axis',(1.,0.,0.));
#8279=DIRECTION('center_axis',(0.,0.,1.));
#8280=DIRECTION('ref_axis',(1.,0.,0.));
#8281=DIRECTION('',(0.,0.,1.));
#8282=DIRECTION('center_axis',(0.,0.,-1.));
#8283=DIRECTION('ref_axis',(1.,0.,0.));
#8284=DIRECTION('center_axis',(0.,0.,1.));
#8285=DIRECTION('ref_axis',(1.,0.,0.));
#8286=DIRECTION('center_axis',(0.,0.,1.));
#8287=DIRECTION('ref_axis',(1.,0.,0.));
#8288=DIRECTION('',(0.,0.,-1.));
#8289=DIRECTION('center_axis',(0.,0.,1.));
#8290=DIRECTION('ref_axis',(1.,0.,0.));
#8291=DIRECTION('center_axis',(0.,0.,1.));
#8292=DIRECTION('ref_axis',(1.,0.,0.));
#8293=DIRECTION('center_axis',(0.,0.,-1.));
#8294=DIRECTION('ref_axis',(1.,0.,0.));
#8295=DIRECTION('center_axis',(0.,0.,1.));
#8296=DIRECTION('ref_axis',(1.,0.,0.));
#8297=DIRECTION('center_axis',(0.,0.,-1.));
#8298=DIRECTION('ref_axis',(1.,0.,0.));
#8299=DIRECTION('',(0.,0.,-1.));
#8300=DIRECTION('center_axis',(0.,0.,1.));
#8301=DIRECTION('ref_axis',(1.,0.,0.));
#8302=DIRECTION('center_axis',(0.,0.,1.));
#8303=DIRECTION('ref_axis',(1.,0.,0.));
#8304=DIRECTION('',(0.,0.,-1.));
#8305=DIRECTION('center_axis',(0.,0.,1.));
#8306=DIRECTION('ref_axis',(1.,0.,0.));
#8307=DIRECTION('center_axis',(0.,0.,1.));
#8308=DIRECTION('ref_axis',(1.,0.,0.));
#8309=DIRECTION('center_axis',(0.,0.,1.));
#8310=DIRECTION('ref_axis',(1.,0.,0.));
#8311=DIRECTION('axis',(0.,0.,1.));
#8312=DIRECTION('refdir',(1.,0.,0.));
#8313=DIRECTION('center_axis',(1.,0.,0.));
#8314=DIRECTION('ref_axis',(0.,0.,-1.));
#8315=DIRECTION('',(1.,0.,0.));
#8316=DIRECTION('center_axis',(0.,0.,1.));
#8317=DIRECTION('ref_axis',(1.,0.,0.));
#8318=DIRECTION('center_axis',(0.,0.,1.));
#8319=DIRECTION('ref_axis',(1.,0.,0.));
#8320=DIRECTION('',(0.,0.,-1.));
#8321=DIRECTION('',(0.,0.,-1.));
#8322=DIRECTION('center_axis',(0.,0.,-1.));
#8323=DIRECTION('ref_axis',(1.,0.,0.));
#8324=DIRECTION('center_axis',(0.,0.,-1.));
#8325=DIRECTION('ref_axis',(1.,0.,0.));
#8326=DIRECTION('center_axis',(0.,0.,-1.));
#8327=DIRECTION('ref_axis',(1.,0.,0.));
#8328=DIRECTION('center_axis',(0.,0.,1.));
#8329=DIRECTION('ref_axis',(1.,0.,0.));
#8330=DIRECTION('center_axis',(0.,0.,1.));
#8331=DIRECTION('ref_axis',(1.,0.,0.));
#8332=DIRECTION('',(-1.,0.,0.));
#8333=DIRECTION('',(0.,-1.,0.));
#8334=DIRECTION('center_axis',(0.,0.,1.));
#8335=DIRECTION('ref_axis',(1.,0.,0.));
#8336=DIRECTION('',(0.,1.,0.));
#8337=DIRECTION('',(-1.,0.,0.));
#8338=DIRECTION('center_axis',(0.,0.,1.));
#8339=DIRECTION('ref_axis',(1.,0.,0.));
#8340=DIRECTION('',(0.,-1.,0.));
#8341=DIRECTION('',(1.,0.,0.));
#8342=DIRECTION('',(0.,1.,0.));
#8343=DIRECTION('center_axis',(0.,1.,0.));
#8344=DIRECTION('ref_axis',(-1.,0.,0.));
#8345=DIRECTION('',(-1.,0.,0.));
#8346=DIRECTION('',(0.,0.,1.));
#8347=DIRECTION('',(0.,0.,1.));
#8348=DIRECTION('center_axis',(1.,0.,0.));
#8349=DIRECTION('ref_axis',(0.,1.,0.));
#8350=DIRECTION('',(0.,1.,0.));
#8351=DIRECTION('',(0.,0.,1.));
#8352=DIRECTION('center_axis',(0.,-1.,0.));
#8353=DIRECTION('ref_axis',(1.,0.,0.));
#8354=DIRECTION('',(1.,0.,0.));
#8355=DIRECTION('',(0.,0.,1.));
#8356=DIRECTION('center_axis',(-1.,0.,0.));
#8357=DIRECTION('ref_axis',(0.,-1.,0.));
#8358=DIRECTION('',(0.,-1.,0.));
#8359=DIRECTION('center_axis',(0.,0.,1.));
#8360=DIRECTION('ref_axis',(1.,0.,0.));
#8361=DIRECTION('axis',(0.,0.,1.));
#8362=DIRECTION('refdir',(1.,0.,0.));
#8363=DIRECTION('axis',(0.,0.,1.));
#8364=DIRECTION('refdir',(1.,0.,0.));
#8365=DIRECTION('center_axis',(0.,-1.,0.));
#8366=DIRECTION('ref_axis',(0.,0.,-1.));
#8367=DIRECTION('center_axis',(0.,-1.,0.));
#8368=DIRECTION('ref_axis',(1.,0.,0.));
#8369=DIRECTION('center_axis',(0.,-1.,0.));
#8370=DIRECTION('ref_axis',(1.,0.,0.));
#8371=DIRECTION('center_axis',(1.,0.,1.22464679914735E-16));
#8372=DIRECTION('ref_axis',(-1.22464679914735E-16,0.,1.));
#8373=DIRECTION('center_axis',(0.,1.,0.));
#8374=DIRECTION('ref_axis',(1.,0.,0.));
#8375=DIRECTION('center_axis',(0.,1.,0.));
#8376=DIRECTION('ref_axis',(1.,0.,0.));
#8377=DIRECTION('center_axis',(0.,-1.,0.));
#8378=DIRECTION('ref_axis',(1.,0.,0.));
#8379=DIRECTION('',(0.,1.,0.));
#8380=DIRECTION('center_axis',(0.,-1.,0.));
#8381=DIRECTION('ref_axis',(1.,0.,0.));
#8382=DIRECTION('center_axis',(0.,-1.,0.));
#8383=DIRECTION('ref_axis',(1.,0.,0.));
#8384=DIRECTION('center_axis',(0.,-1.,0.));
#8385=DIRECTION('ref_axis',(1.,0.,0.));
#8386=DIRECTION('',(0.,1.,0.));
#8387=DIRECTION('center_axis',(0.,-1.,0.));
#8388=DIRECTION('ref_axis',(1.,0.,0.));
#8389=DIRECTION('center_axis',(0.,1.,0.));
#8390=DIRECTION('ref_axis',(1.,0.,0.));
#8391=DIRECTION('',(-0.707106781186547,0.707106781186548,-8.65956056235493E-17));
#8392=DIRECTION('center_axis',(0.,-1.,0.));
#8393=DIRECTION('ref_axis',(1.,0.,0.));
#8394=DIRECTION('center_axis',(0.,1.,0.));
#8395=DIRECTION('ref_axis',(0.,0.,1.));
#8396=DIRECTION('center_axis',(0.,-1.,0.));
#8397=DIRECTION('ref_axis',(1.,0.,0.));
#8398=DIRECTION('center_axis',(0.,-1.,0.));
#8399=DIRECTION('ref_axis',(1.,0.,0.));
#8400=DIRECTION('',(0.,1.,0.));
#8401=DIRECTION('center_axis',(0.,-1.,0.));
#8402=DIRECTION('ref_axis',(0.,0.,-1.));
#8403=DIRECTION('center_axis',(0.,-1.,0.));
#8404=DIRECTION('ref_axis',(1.,0.,0.));
#8405=DIRECTION('center_axis',(0.,-1.,0.));
#8406=DIRECTION('ref_axis',(1.,0.,0.));
#8407=DIRECTION('',(0.707106781186547,0.707106781186548,8.65956056235493E-17));
#8408=DIRECTION('axis',(0.,0.,1.));
#8409=DIRECTION('refdir',(1.,0.,0.));
#8410=DIRECTION('center_axis',(0.,-1.,0.));
#8411=DIRECTION('ref_axis',(0.,0.,-1.));
#8412=DIRECTION('center_axis',(0.,-1.,0.));
#8413=DIRECTION('ref_axis',(1.,0.,0.));
#8414=DIRECTION('center_axis',(0.,-1.,0.));
#8415=DIRECTION('ref_axis',(1.,0.,0.));
#8416=DIRECTION('center_axis',(1.,0.,1.22464679914735E-16));
#8417=DIRECTION('ref_axis',(-1.22464679914735E-16,0.,1.));
#8418=DIRECTION('center_axis',(0.,1.,0.));
#8419=DIRECTION('ref_axis',(1.,0.,0.));
#8420=DIRECTION('center_axis',(0.,1.,0.));
#8421=DIRECTION('ref_axis',(1.,0.,0.));
#8422=DIRECTION('center_axis',(0.,-1.,0.));
#8423=DIRECTION('ref_axis',(1.,0.,0.));
#8424=DIRECTION('center_axis',(0.,-1.,0.));
#8425=DIRECTION('ref_axis',(1.,0.,0.));
#8426=DIRECTION('',(0.,1.,0.));
#8427=DIRECTION('center_axis',(0.,1.,0.));
#8428=DIRECTION('ref_axis',(0.,0.,1.));
#8429=DIRECTION('center_axis',(0.,-1.,0.));
#8430=DIRECTION('ref_axis',(1.,0.,0.));
#8431=DIRECTION('center_axis',(0.,-1.,0.));
#8432=DIRECTION('ref_axis',(1.,0.,0.));
#8433=DIRECTION('center_axis',(0.,-1.,0.));
#8434=DIRECTION('ref_axis',(1.,0.,0.));
#8435=DIRECTION('center_axis',(0.,-1.,0.));
#8436=DIRECTION('ref_axis',(1.,0.,0.));
#8437=DIRECTION('',(0.707106781186548,0.707106781186547,8.65956056235494E-17));
#8438=DIRECTION('center_axis',(0.,-1.,0.));
#8439=DIRECTION('ref_axis',(1.,0.,0.));
#8440=DIRECTION('center_axis',(0.,-1.,0.));
#8441=DIRECTION('ref_axis',(1.,0.,0.));
#8442=DIRECTION('',(0.,1.,0.));
#8443=DIRECTION('center_axis',(0.,1.,0.));
#8444=DIRECTION('ref_axis',(1.,0.,0.));
#8445=DIRECTION('center_axis',(0.,-1.,0.));
#8446=DIRECTION('ref_axis',(1.,0.,0.));
#8447=DIRECTION('',(-0.707106781186548,0.707106781186547,-8.65956056235494E-17));
#8448=DIRECTION('center_axis',(0.,-1.,0.));
#8449=DIRECTION('ref_axis',(0.,0.,-1.));
#8450=DIRECTION('center_axis',(0.,-1.,0.));
#8451=DIRECTION('ref_axis',(1.,0.,0.));
#8452=DIRECTION('',(0.,1.,0.));
#8453=DIRECTION('axis',(0.,0.,1.));
#8454=DIRECTION('refdir',(1.,0.,0.));
#8455=DIRECTION('center_axis',(0.,0.,1.));
#8456=DIRECTION('ref_axis',(1.,0.,0.));
#8457=DIRECTION('center_axis',(1.22464679914735E-16,-1.,0.));
#8458=DIRECTION('ref_axis',(-1.,-1.22464679914735E-16,0.));
#8459=DIRECTION('center_axis',(0.707106781186548,0.,0.707106781186548));
#8460=DIRECTION('ref_axis',(0.707106781186548,0.,-0.707106781186548));
#8461=DIRECTION('center_axis',(8.65956056235494E-17,-1.,-8.65956056235493E-17));
#8462=DIRECTION('ref_axis',(-0.707106781186547,-1.22464679914735E-16,0.707106781186547));
#8463=DIRECTION('center_axis',(1.,0.,0.));
#8464=DIRECTION('ref_axis',(6.12323399573676E-17,0.,-1.));
#8465=DIRECTION('center_axis',(7.49879891330929E-33,-1.,-1.22464679914735E-16));
#8466=DIRECTION('ref_axis',(-6.12323399573676E-17,-1.22464679914735E-16,
1.));
#8467=DIRECTION('center_axis',(0.707106781186548,0.,-0.707106781186548));
#8468=DIRECTION('ref_axis',(-0.707106781186548,0.,-0.707106781186548));
#8469=DIRECTION('center_axis',(-8.65956056235493E-17,-1.,-8.65956056235494E-17));
#8470=DIRECTION('ref_axis',(0.707106781186547,-1.22464679914735E-16,0.707106781186547));
#8471=DIRECTION('center_axis',(0.,0.,-1.));
#8472=DIRECTION('ref_axis',(-1.,0.,-1.22464679914735E-16));
#8473=DIRECTION('center_axis',(-1.22464679914735E-16,-1.,-1.49975978266186E-32));
#8474=DIRECTION('ref_axis',(1.,-1.22464679914735E-16,1.22464679914735E-16));
#8475=DIRECTION('center_axis',(-0.707106781186547,0.,-0.707106781186548));
#8476=DIRECTION('ref_axis',(-0.707106781186548,0.,0.707106781186547));
#8477=DIRECTION('center_axis',(-8.65956056235493E-17,-1.,8.65956056235493E-17));
#8478=DIRECTION('ref_axis',(0.707106781186548,-1.22464679914735E-16,-0.707106781186547));
#8479=DIRECTION('center_axis',(-1.,0.,0.));
#8480=DIRECTION('ref_axis',(-1.83697019872103E-16,0.,1.));
#8481=DIRECTION('center_axis',(-2.24963967399279E-32,-1.,1.22464679914735E-16));
#8482=DIRECTION('ref_axis',(1.83697019872103E-16,-1.22464679914735E-16,
-1.));
#8483=DIRECTION('center_axis',(-0.707106781186548,0.,0.707106781186548));
#8484=DIRECTION('ref_axis',(0.707106781186547,0.,0.707106781186548));
#8485=DIRECTION('center_axis',(8.65956056235493E-17,-1.,8.65956056235493E-17));
#8486=DIRECTION('ref_axis',(-0.707106781186547,-1.22464679914735E-16,-0.707106781186548));
#8487=DIRECTION('axis',(0.,0.,1.));
#8488=DIRECTION('refdir',(1.,0.,0.));
#8489=DIRECTION('center_axis',(0.,0.,1.));
#8490=DIRECTION('ref_axis',(1.,0.,0.));
#8491=DIRECTION('center_axis',(0.,-1.,0.));
#8492=DIRECTION('ref_axis',(0.,0.,-1.));
#8493=DIRECTION('center_axis',(0.,-1.,0.));
#8494=DIRECTION('ref_axis',(0.,0.,-1.));
#8495=DIRECTION('center_axis',(0.,1.,0.));
#8496=DIRECTION('ref_axis',(1.,0.,0.));
#8497=DIRECTION('center_axis',(0.,1.,0.));
#8498=DIRECTION('ref_axis',(1.,0.,0.));
#8499=DIRECTION('center_axis',(0.,1.,0.));
#8500=DIRECTION('ref_axis',(1.,0.,0.));
#8501=DIRECTION('center_axis',(0.,1.,0.));
#8502=DIRECTION('ref_axis',(1.,0.,0.));
#8503=DIRECTION('',(0.,-1.,0.));
#8504=DIRECTION('center_axis',(0.,-1.,0.));
#8505=DIRECTION('ref_axis',(1.,0.,0.));
#8506=DIRECTION('center_axis',(0.,1.,0.));
#8507=DIRECTION('ref_axis',(1.,0.,0.));
#8508=DIRECTION('center_axis',(0.,1.,0.));
#8509=DIRECTION('ref_axis',(1.,0.,0.));
#8510=DIRECTION('center_axis',(0.,1.,0.));
#8511=DIRECTION('ref_axis',(1.,0.,0.));
#8512=DIRECTION('center_axis',(0.,1.,0.));
#8513=DIRECTION('ref_axis',(1.,0.,0.));
#8514=DIRECTION('center_axis',(0.,1.,0.));
#8515=DIRECTION('ref_axis',(1.,0.,0.));
#8516=DIRECTION('center_axis',(0.,1.,0.));
#8517=DIRECTION('ref_axis',(1.,0.,0.));
#8518=DIRECTION('center_axis',(0.,-1.,0.));
#8519=DIRECTION('ref_axis',(1.,0.,0.));
#8520=DIRECTION('center_axis',(0.,-1.,0.));
#8521=DIRECTION('ref_axis',(0.,0.,-1.));
#8522=DIRECTION('center_axis',(6.12323399573677E-17,0.,1.));
#8523=DIRECTION('ref_axis',(1.,0.,0.));
#8524=DIRECTION('center_axis',(0.,-1.,0.));
#8525=DIRECTION('ref_axis',(0.,0.,-1.));
#8526=DIRECTION('center_axis',(0.,1.,0.));
#8527=DIRECTION('ref_axis',(1.,0.,0.));
#8528=DIRECTION('center_axis',(0.,-1.,0.));
#8529=DIRECTION('ref_axis',(1.,0.,0.));
#8530=DIRECTION('center_axis',(0.,-1.,0.));
#8531=DIRECTION('ref_axis',(0.,0.,-1.));
#8532=DIRECTION('center_axis',(0.,0.,1.));
#8533=DIRECTION('ref_axis',(1.,0.,0.));
#8534=DIRECTION('center_axis',(0.,-1.,0.));
#8535=DIRECTION('ref_axis',(0.,0.,-1.));
#8536=DIRECTION('center_axis',(0.,1.,0.));
#8537=DIRECTION('ref_axis',(1.,0.,0.));
#8538=DIRECTION('center_axis',(0.,-1.,0.));
#8539=DIRECTION('ref_axis',(1.,0.,0.));
#8540=DIRECTION('center_axis',(0.,-1.,0.));
#8541=DIRECTION('ref_axis',(0.,0.,-1.));
#8542=DIRECTION('center_axis',(0.,0.,1.));
#8543=DIRECTION('ref_axis',(1.,0.,0.));
#8544=DIRECTION('center_axis',(0.,-1.,0.));
#8545=DIRECTION('ref_axis',(0.,0.,-1.));
#8546=DIRECTION('center_axis',(0.,1.,0.));
#8547=DIRECTION('ref_axis',(1.,0.,0.));
#8548=DIRECTION('center_axis',(0.,-1.,0.));
#8549=DIRECTION('ref_axis',(1.,0.,0.));
#8550=DIRECTION('center_axis',(0.,-1.,0.));
#8551=DIRECTION('ref_axis',(0.,0.,-1.));
#8552=DIRECTION('center_axis',(0.,0.,1.));
#8553=DIRECTION('ref_axis',(1.,0.,0.));
#8554=DIRECTION('center_axis',(0.,-1.,0.));
#8555=DIRECTION('ref_axis',(0.,0.,-1.));
#8556=DIRECTION('center_axis',(0.,1.,0.));
#8557=DIRECTION('ref_axis',(1.,0.,0.));
#8558=DIRECTION('center_axis',(0.,-1.,0.));
#8559=DIRECTION('ref_axis',(1.,0.,0.));
#8560=DIRECTION('center_axis',(0.,-1.,0.));
#8561=DIRECTION('ref_axis',(0.,0.,-1.));
#8562=DIRECTION('center_axis',(6.12323399573676E-17,0.,1.));
#8563=DIRECTION('ref_axis',(1.,0.,0.));
#8564=DIRECTION('center_axis',(0.,-1.,0.));
#8565=DIRECTION('ref_axis',(0.,0.,-1.));
#8566=DIRECTION('center_axis',(0.,1.,0.));
#8567=DIRECTION('ref_axis',(1.,0.,0.));
#8568=DIRECTION('center_axis',(0.,-1.,0.));
#8569=DIRECTION('ref_axis',(1.,0.,0.));
#8570=DIRECTION('center_axis',(0.,-1.,0.));
#8571=DIRECTION('ref_axis',(0.,0.,-1.));
#8572=DIRECTION('center_axis',(0.,0.,1.));
#8573=DIRECTION('ref_axis',(1.,0.,0.));
#8574=DIRECTION('center_axis',(0.,-1.,0.));
#8575=DIRECTION('ref_axis',(0.,0.,-1.));
#8576=DIRECTION('center_axis',(0.,1.,0.));
#8577=DIRECTION('ref_axis',(1.,0.,0.));
#8578=DIRECTION('center_axis',(0.,1.,0.));
#8579=DIRECTION('ref_axis',(1.,0.,0.));
#8580=DIRECTION('',(0.,1.,0.));
#8581=DIRECTION('center_axis',(0.,-1.,0.));
#8582=DIRECTION('ref_axis',(1.,0.,0.));
#8583=DIRECTION('center_axis',(0.,-1.,0.));
#8584=DIRECTION('ref_axis',(1.,0.,0.));
#8585=DIRECTION('center_axis',(0.,1.,0.));
#8586=DIRECTION('ref_axis',(1.,0.,0.));
#8587=DIRECTION('center_axis',(0.,-1.,0.));
#8588=DIRECTION('ref_axis',(0.,0.,-1.));
#8589=DIRECTION('center_axis',(0.,0.,1.));
#8590=DIRECTION('ref_axis',(1.,0.,0.));
#8591=DIRECTION('center_axis',(0.,-1.,0.));
#8592=DIRECTION('ref_axis',(0.,0.,-1.));
#8593=DIRECTION('center_axis',(0.,-1.,0.));
#8594=DIRECTION('ref_axis',(-1.,0.,0.));
#8595=DIRECTION('center_axis',(0.,1.,0.));
#8596=DIRECTION('ref_axis',(1.,0.,0.));
#8597=DIRECTION('axis',(0.,0.,1.));
#8598=DIRECTION('refdir',(1.,0.,0.));
#8599=DIRECTION('center_axis',(0.,1.,0.));
#8600=DIRECTION('ref_axis',(0.,0.,1.));
#8601=DIRECTION('center_axis',(0.,-1.,0.));
#8602=DIRECTION('ref_axis',(1.,0.,0.));
#8603=DIRECTION('center_axis',(0.,-1.,0.));
#8604=DIRECTION('ref_axis',(1.,0.,0.));
#8605=DIRECTION('center_axis',(0.,-1.,0.));
#8606=DIRECTION('ref_axis',(1.,0.,0.));
#8607=DIRECTION('center_axis',(0.,-1.,0.));
#8608=DIRECTION('ref_axis',(1.,0.,0.));
#8609=DIRECTION('',(0.,1.,0.));
#8610=DIRECTION('center_axis',(0.,-1.,0.));
#8611=DIRECTION('ref_axis',(0.,0.,-1.));
#8612=DIRECTION('center_axis',(0.,-1.,0.));
#8613=DIRECTION('ref_axis',(1.,0.,0.));
#8614=DIRECTION('center_axis',(0.,-1.,0.));
#8615=DIRECTION('ref_axis',(1.,0.,0.));
#8616=DIRECTION('',(0.,1.,0.));
#8617=DIRECTION('center_axis',(0.,1.,0.));
#8618=DIRECTION('ref_axis',(0.,0.,1.));
#8619=DIRECTION('center_axis',(0.,-1.,0.));
#8620=DIRECTION('ref_axis',(1.,0.,0.));
#8621=DIRECTION('center_axis',(0.,-1.,0.));
#8622=DIRECTION('ref_axis',(1.,0.,0.));
#8623=DIRECTION('center_axis',(0.,-1.,0.));
#8624=DIRECTION('ref_axis',(1.,0.,0.));
#8625=DIRECTION('center_axis',(0.,-1.,0.));
#8626=DIRECTION('ref_axis',(1.,0.,0.));
#8627=DIRECTION('',(0.,1.,0.));
#8628=DIRECTION('center_axis',(0.,-1.,0.));
#8629=DIRECTION('ref_axis',(0.,0.,-1.));
#8630=DIRECTION('center_axis',(0.,-1.,0.));
#8631=DIRECTION('ref_axis',(1.,0.,0.));
#8632=DIRECTION('center_axis',(0.,-1.,0.));
#8633=DIRECTION('ref_axis',(1.,0.,0.));
#8634=DIRECTION('',(0.,1.,0.));
#8635=DIRECTION('',(0.,0.,1.));
#8636=DIRECTION('',(1.,0.,0.));
#8637=DIRECTION('',(0.,0.,1.));
#8638=DIRECTION('',(1.,0.,0.));
#8639=DIRECTION('',(0.,0.,1.));
#8640=DIRECTION('',(1.,0.,0.));
#8641=DIRECTION('',(0.,0.,1.));
#8642=DIRECTION('',(1.,0.,0.));
#8643=DIRECTION('',(0.,0.,1.));
#8644=DIRECTION('',(1.,0.,0.));
#8645=DIRECTION('axis',(0.,0.,1.));
#8646=DIRECTION('refdir',(1.,0.,0.));
#8647=DIRECTION('center_axis',(0.,1.,0.));
#8648=DIRECTION('ref_axis',(1.,0.,0.));
#8649=DIRECTION('center_axis',(0.,1.,0.));
#8650=DIRECTION('ref_axis',(1.,0.,0.));
#8651=DIRECTION('center_axis',(0.,1.,0.));
#8652=DIRECTION('ref_axis',(0.,0.,1.));
#8653=DIRECTION('center_axis',(0.,-1.,0.));
#8654=DIRECTION('ref_axis',(1.,0.,0.));
#8655=DIRECTION('center_axis',(0.,-1.,0.));
#8656=DIRECTION('ref_axis',(1.,0.,0.));
#8657=DIRECTION('center_axis',(0.,-1.,0.));
#8658=DIRECTION('ref_axis',(1.,0.,0.));
#8659=DIRECTION('',(0.707106781186547,0.707106781186548,8.65956056235493E-17));
#8660=DIRECTION('center_axis',(0.,-1.,0.));
#8661=DIRECTION('ref_axis',(1.,0.,0.));
#8662=DIRECTION('center_axis',(0.,-1.,0.));
#8663=DIRECTION('ref_axis',(1.,0.,0.));
#8664=DIRECTION('',(0.,1.,0.));
#8665=DIRECTION('center_axis',(0.,1.,0.));
#8666=DIRECTION('ref_axis',(1.,0.,0.));
#8667=DIRECTION('center_axis',(0.,-1.,0.));
#8668=DIRECTION('ref_axis',(1.,0.,0.));
#8669=DIRECTION('',(-0.707106781186547,0.707106781186548,-8.65956056235493E-17));
#8670=DIRECTION('center_axis',(0.,-1.,0.));
#8671=DIRECTION('ref_axis',(0.,0.,-1.));
#8672=DIRECTION('center_axis',(0.,-1.,0.));
#8673=DIRECTION('ref_axis',(1.,0.,0.));
#8674=DIRECTION('center_axis',(0.,1.,0.));
#8675=DIRECTION('ref_axis',(1.,0.,0.));
#8676=DIRECTION('center_axis',(0.,1.,0.));
#8677=DIRECTION('ref_axis',(1.,0.,0.));
#8678=DIRECTION('',(-0.447213595499958,0.894427190999916,-5.47678698264203E-17));
#8679=DIRECTION('center_axis',(0.,-1.,0.));
#8680=DIRECTION('ref_axis',(1.,0.,0.));
#8681=DIRECTION('',(0.,1.,0.));
#8682=DIRECTION('center_axis',(0.866025403784439,0.,-0.5));
#8683=DIRECTION('ref_axis',(0.5,0.,0.866025403784439));
#8684=DIRECTION('',(-0.5,0.,-0.866025403784439));
#8685=DIRECTION('',(0.,-1.,0.));
#8686=DIRECTION('',(0.5,0.,0.866025403784439));
#8687=DIRECTION('',(0.,-1.,0.));
#8688=DIRECTION('center_axis',(1.60246890531964E-16,0.,-1.));
#8689=DIRECTION('ref_axis',(1.,0.,1.60246890531964E-16));
#8690=DIRECTION('',(-1.,0.,-1.60246890531964E-16));
#8691=DIRECTION('',(0.,-1.,0.));
#8692=DIRECTION('',(1.,0.,1.60246890531964E-16));
#8693=DIRECTION('center_axis',(-0.866025403784439,0.,-0.5));
#8694=DIRECTION('ref_axis',(0.5,0.,-0.866025403784439));
#8695=DIRECTION('',(-0.5,0.,0.866025403784439));
#8696=DIRECTION('',(0.,-1.,0.));
#8697=DIRECTION('',(0.5,0.,-0.866025403784439));
#8698=DIRECTION('center_axis',(-0.866025403784439,0.,0.5));
#8699=DIRECTION('ref_axis',(-0.5,0.,-0.866025403784439));
#8700=DIRECTION('',(0.5,0.,0.866025403784439));
#8701=DIRECTION('',(0.,-1.,0.));
#8702=DIRECTION('',(-0.5,0.,-0.866025403784439));
#8703=DIRECTION('center_axis',(-1.60246890531964E-16,0.,1.));
#8704=DIRECTION('ref_axis',(-1.,0.,-1.60246890531964E-16));
#8705=DIRECTION('',(1.,0.,1.60246890531964E-16));
#8706=DIRECTION('',(0.,-1.,0.));
#8707=DIRECTION('',(-1.,0.,-1.60246890531964E-16));
#8708=DIRECTION('center_axis',(0.866025403784439,0.,0.5));
#8709=DIRECTION('ref_axis',(-0.5,0.,0.866025403784439));
#8710=DIRECTION('',(0.5,0.,-0.866025403784439));
#8711=DIRECTION('',(-0.5,0.,0.866025403784439));
#8712=DIRECTION('center_axis',(0.,1.,0.));
#8713=DIRECTION('ref_axis',(1.,0.,0.));
#8714=DIRECTION('center_axis',(0.,-1.,0.));
#8715=DIRECTION('ref_axis',(0.,0.,-1.));
#8716=DIRECTION('',(0.,0.,1.));
#8717=DIRECTION('',(1.,0.,0.));
#8718=DIRECTION('',(0.,0.,1.));
#8719=DIRECTION('',(1.,0.,0.));
#8720=DIRECTION('',(0.,0.,1.));
#8721=DIRECTION('',(1.,0.,0.));
#8722=DIRECTION('',(0.,0.,1.));
#8723=DIRECTION('',(1.,0.,0.));
#8724=DIRECTION('',(0.,0.,1.));
#8725=DIRECTION('',(1.,0.,0.));
#8726=DIRECTION('',(0.,0.,1.));
#8727=DIRECTION('',(1.,0.,0.));
#8728=DIRECTION('',(0.,-1.,2.22044604925031E-16));
#8729=DIRECTION('',(1.,0.,0.));
#8730=DIRECTION('',(0.,1.,2.22044604925031E-16));
#8731=DIRECTION('',(1.,0.,0.));
#8732=DIRECTION('',(0.,1.,2.22044604925031E-16));
#8733=DIRECTION('',(1.,0.,0.));
#8734=DIRECTION('',(0.,1.,2.22044604925031E-16));
#8735=DIRECTION('',(1.,0.,0.));
#8736=DIRECTION('',(0.,1.,2.22044604925031E-16));
#8737=DIRECTION('',(1.,0.,0.));
#8738=DIRECTION('',(0.,-1.,2.22044604925031E-16));
#8739=DIRECTION('',(1.,0.,0.));
#8740=DIRECTION('',(0.,-1.,2.22044604925031E-16));
#8741=DIRECTION('',(1.,0.,0.));
#8742=DIRECTION('',(0.,-1.,2.22044604925031E-16));
#8743=DIRECTION('',(1.,0.,0.));
#8744=DIRECTION('',(0.,-1.,2.22044604925031E-16));
#8745=DIRECTION('',(1.,0.,0.));
#8746=DIRECTION('',(0.,-1.,2.22044604925031E-16));
#8747=DIRECTION('',(1.,0.,0.));
#8748=DIRECTION('',(0.,1.,2.22044604925031E-16));
#8749=DIRECTION('',(1.,0.,0.));
#8750=DIRECTION('',(0.,1.,2.22044604925031E-16));
#8751=DIRECTION('',(1.,0.,0.));
#8752=DIRECTION('',(0.,1.,2.22044604925031E-16));
#8753=DIRECTION('',(1.,0.,0.));
#8754=DIRECTION('',(0.,1.,2.22044604925031E-16));
#8755=DIRECTION('',(1.,0.,0.));
#8756=DIRECTION('',(0.,-1.,2.22044604925031E-16));
#8757=DIRECTION('',(1.,0.,0.));
#8758=DIRECTION('',(0.,-1.,2.22044604925031E-16));
#8759=DIRECTION('',(1.,0.,0.));
#8760=DIRECTION('',(0.,-1.,2.22044604925031E-16));
#8761=DIRECTION('',(1.,0.,0.));
#8762=DIRECTION('',(0.,-1.,2.22044604925031E-16));
#8763=DIRECTION('',(1.,0.,0.));
#8764=DIRECTION('axis',(0.,0.,1.));
#8765=DIRECTION('refdir',(1.,0.,0.));
#8766=DIRECTION('axis',(0.,0.,1.));
#8767=DIRECTION('refdir',(1.,0.,0.));
#8768=DIRECTION('center_axis',(0.,0.,1.));
#8769=DIRECTION('ref_axis',(1.,0.,0.));
#8770=DIRECTION('center_axis',(0.,0.,1.));
#8771=DIRECTION('ref_axis',(1.,0.,0.));
#8772=DIRECTION('',(0.,0.,1.));
#8773=DIRECTION('center_axis',(0.,0.,-1.));
#8774=DIRECTION('ref_axis',(1.,0.,0.));
#8775=DIRECTION('center_axis',(0.,0.,1.));
#8776=DIRECTION('ref_axis',(1.,0.,0.));
#8777=DIRECTION('center_axis',(0.,0.,1.));
#8778=DIRECTION('ref_axis',(1.,0.,0.));
#8779=DIRECTION('center_axis',(0.,0.,1.));
#8780=DIRECTION('ref_axis',(1.,0.,0.));
#8781=DIRECTION('',(0.,0.,-1.));
#8782=DIRECTION('center_axis',(0.,0.,-1.));
#8783=DIRECTION('ref_axis',(1.,0.,0.));
#8784=DIRECTION('center_axis',(0.,0.,1.));
#8785=DIRECTION('ref_axis',(1.,0.,0.));
#8786=DIRECTION('center_axis',(0.,0.,1.));
#8787=DIRECTION('ref_axis',(1.,0.,0.));
#8788=DIRECTION('center_axis',(0.,0.,1.));
#8789=DIRECTION('ref_axis',(1.,0.,0.));
#8790=DIRECTION('center_axis',(0.,0.,-1.));
#8791=DIRECTION('ref_axis',(1.,0.,0.));
#8792=DIRECTION('center_axis',(0.,0.,1.));
#8793=DIRECTION('ref_axis',(1.,0.,0.));
#8794=DIRECTION('center_axis',(0.,0.,1.));
#8795=DIRECTION('ref_axis',(1.,0.,0.));
#8796=DIRECTION('',(0.,0.,-1.));
#8797=DIRECTION('center_axis',(0.,0.,1.));
#8798=DIRECTION('ref_axis',(1.,0.,0.));
#8799=DIRECTION('',(0.,0.,-1.));
#8800=DIRECTION('center_axis',(0.,0.,1.));
#8801=DIRECTION('ref_axis',(1.,0.,0.));
#8802=DIRECTION('center_axis',(0.,0.,1.));
#8803=DIRECTION('ref_axis',(1.,0.,0.));
#8804=DIRECTION('center_axis',(0.,0.,1.));
#8805=DIRECTION('ref_axis',(1.,0.,0.));
#8806=DIRECTION('axis',(0.,0.,1.));
#8807=DIRECTION('refdir',(1.,0.,0.));
#8808=DIRECTION('center_axis',(1.,0.,0.));
#8809=DIRECTION('ref_axis',(0.,0.,-1.));
#8810=DIRECTION('',(0.,0.,1.));
#8811=DIRECTION('center_axis',(1.,0.,0.));
#8812=DIRECTION('ref_axis',(0.,0.,-1.));
#8813=DIRECTION('center_axis',(1.,0.,0.));
#8814=DIRECTION('ref_axis',(0.,0.,-1.));
#8815=DIRECTION('center_axis',(1.,0.,0.));
#8816=DIRECTION('ref_axis',(0.,0.,-1.));
#8817=DIRECTION('',(1.,0.,0.));
#8818=DIRECTION('center_axis',(1.,0.,0.));
#8819=DIRECTION('ref_axis',(0.,0.,-1.));
#8820=DIRECTION('',(0.,0.,-1.));
#8821=DIRECTION('center_axis',(0.,0.,1.));
#8822=DIRECTION('ref_axis',(1.,0.,0.));
#8823=DIRECTION('center_axis',(0.,0.,-1.));
#8824=DIRECTION('ref_axis',(1.,0.,0.));
#8825=DIRECTION('',(0.,0.,-1.));
#8826=DIRECTION('center_axis',(0.,0.,-1.));
#8827=DIRECTION('ref_axis',(1.,0.,0.));
#8828=DIRECTION('center_axis',(0.,0.,1.));
#8829=DIRECTION('ref_axis',(1.,0.,0.));
#8830=DIRECTION('center_axis',(0.,0.,1.));
#8831=DIRECTION('ref_axis',(1.,0.,0.));
#8832=DIRECTION('',(0.,0.,-1.));
#8833=DIRECTION('center_axis',(0.,0.,1.));
#8834=DIRECTION('ref_axis',(1.,0.,0.));
#8835=DIRECTION('center_axis',(0.,0.,1.));
#8836=DIRECTION('ref_axis',(1.,0.,0.));
#8837=DIRECTION('center_axis',(0.,0.,1.));
#8838=DIRECTION('ref_axis',(1.,0.,0.));
#8839=DIRECTION('axis',(0.,0.,1.));
#8840=DIRECTION('refdir',(1.,0.,0.));
#8841=DIRECTION('center_axis',(0.,0.,1.));
#8842=DIRECTION('ref_axis',(1.,0.,0.));
#8843=DIRECTION('center_axis',(0.,0.,-1.));
#8844=DIRECTION('ref_axis',(1.,0.,0.));
#8845=DIRECTION('',(0.,0.,-1.));
#8846=DIRECTION('center_axis',(0.,0.,-1.));
#8847=DIRECTION('ref_axis',(1.,0.,0.));
#8848=DIRECTION('center_axis',(0.,0.,1.));
#8849=DIRECTION('ref_axis',(1.,0.,0.));
#8850=DIRECTION('center_axis',(0.,0.,1.));
#8851=DIRECTION('ref_axis',(1.,0.,0.));
#8852=DIRECTION('',(0.,0.,-1.));
#8853=DIRECTION('center_axis',(0.,0.,1.));
#8854=DIRECTION('ref_axis',(1.,0.,0.));
#8855=DIRECTION('center_axis',(0.,0.,1.));
#8856=DIRECTION('ref_axis',(1.,0.,0.));
#8857=DIRECTION('center_axis',(0.,0.,1.));
#8858=DIRECTION('ref_axis',(1.,0.,0.));
#8859=DIRECTION('axis',(0.,0.,1.));
#8860=DIRECTION('refdir',(1.,0.,0.));
#8861=DIRECTION('center_axis',(0.,0.,1.));
#8862=DIRECTION('ref_axis',(1.,0.,0.));
#8863=DIRECTION('center_axis',(0.,0.,-1.));
#8864=DIRECTION('ref_axis',(1.,0.,0.));
#8865=DIRECTION('',(0.,0.,-1.));
#8866=DIRECTION('center_axis',(0.,0.,-1.));
#8867=DIRECTION('ref_axis',(1.,0.,0.));
#8868=DIRECTION('center_axis',(0.,0.,1.));
#8869=DIRECTION('ref_axis',(1.,0.,0.));
#8870=DIRECTION('center_axis',(0.,0.,1.));
#8871=DIRECTION('ref_axis',(1.,0.,0.));
#8872=DIRECTION('',(0.,0.,-1.));
#8873=DIRECTION('center_axis',(0.,0.,1.));
#8874=DIRECTION('ref_axis',(1.,0.,0.));
#8875=DIRECTION('center_axis',(0.,0.,1.));
#8876=DIRECTION('ref_axis',(1.,0.,0.));
#8877=DIRECTION('center_axis',(0.,0.,1.));
#8878=DIRECTION('ref_axis',(1.,0.,0.));
#8879=DIRECTION('axis',(0.,0.,1.));
#8880=DIRECTION('refdir',(1.,0.,0.));
#8881=DIRECTION('center_axis',(1.,0.,0.));
#8882=DIRECTION('ref_axis',(0.,0.,-1.));
#8883=DIRECTION('center_axis',(1.,0.,0.));
#8884=DIRECTION('ref_axis',(0.,0.,-1.));
#8885=DIRECTION('',(-1.,0.,0.));
#8886=DIRECTION('center_axis',(1.,0.,0.));
#8887=DIRECTION('ref_axis',(0.,0.,-1.));
#8888=DIRECTION('center_axis',(1.,0.,0.));
#8889=DIRECTION('ref_axis',(0.,0.,-1.));
#8890=DIRECTION('center_axis',(1.,0.,0.));
#8891=DIRECTION('ref_axis',(0.,0.,-1.));
#8892=DIRECTION('axis',(0.,0.,1.));
#8893=DIRECTION('refdir',(1.,0.,0.));
#8894=DIRECTION('center_axis',(1.,0.,0.));
#8895=DIRECTION('ref_axis',(0.,0.,-1.));
#8896=DIRECTION('center_axis',(1.,0.,0.));
#8897=DIRECTION('ref_axis',(0.,0.,-1.));
#8898=DIRECTION('',(-1.,0.,0.));
#8899=DIRECTION('center_axis',(1.,0.,0.));
#8900=DIRECTION('ref_axis',(0.,0.,-1.));
#8901=DIRECTION('center_axis',(1.,0.,0.));
#8902=DIRECTION('ref_axis',(0.,0.,-1.));
#8903=DIRECTION('center_axis',(1.,0.,0.));
#8904=DIRECTION('ref_axis',(0.,0.,-1.));
#8905=DIRECTION('axis',(0.,0.,1.));
#8906=DIRECTION('refdir',(1.,0.,0.));
#8907=DIRECTION('center_axis',(0.,0.,1.));
#8908=DIRECTION('ref_axis',(1.,0.,0.));
#8909=DIRECTION('center_axis',(0.,0.,-1.));
#8910=DIRECTION('ref_axis',(1.,0.,0.));
#8911=DIRECTION('',(0.,0.,-1.));
#8912=DIRECTION('center_axis',(0.,0.,-1.));
#8913=DIRECTION('ref_axis',(1.,0.,0.));
#8914=DIRECTION('center_axis',(0.,0.,1.));
#8915=DIRECTION('ref_axis',(1.,0.,0.));
#8916=DIRECTION('center_axis',(0.,0.,1.));
#8917=DIRECTION('ref_axis',(1.,0.,0.));
#8918=DIRECTION('',(0.,0.,-1.));
#8919=DIRECTION('center_axis',(0.,0.,1.));
#8920=DIRECTION('ref_axis',(1.,0.,0.));
#8921=DIRECTION('center_axis',(0.,0.,1.));
#8922=DIRECTION('ref_axis',(1.,0.,0.));
#8923=DIRECTION('center_axis',(0.,0.,1.));
#8924=DIRECTION('ref_axis',(1.,0.,0.));
#8925=DIRECTION('axis',(0.,0.,1.));
#8926=DIRECTION('refdir',(1.,0.,0.));
#8927=DIRECTION('center_axis',(0.,1.,0.));
#8928=DIRECTION('ref_axis',(1.,0.,0.));
#8929=DIRECTION('center_axis',(0.,1.,0.));
#8930=DIRECTION('ref_axis',(1.,0.,0.));
#8931=DIRECTION('center_axis',(0.866025403784439,0.,-0.5));
#8932=DIRECTION('ref_axis',(0.5,0.,0.866025403784439));
#8933=DIRECTION('',(0.5,0.,0.866025403784439));
#8934=DIRECTION('',(0.,-1.,0.));
#8935=DIRECTION('',(0.5,0.,0.866025403784439));
#8936=DIRECTION('',(0.,-1.,0.));
#8937=DIRECTION('center_axis',(1.20185167898973E-16,0.,-1.));
#8938=DIRECTION('ref_axis',(1.,0.,1.20185167898973E-16));
#8939=DIRECTION('',(1.,0.,1.20185167898973E-16));
#8940=DIRECTION('',(0.,-1.,0.));
#8941=DIRECTION('',(1.,0.,1.20185167898973E-16));
#8942=DIRECTION('center_axis',(-0.866025403784439,0.,-0.5));
#8943=DIRECTION('ref_axis',(0.5,0.,-0.866025403784439));
#8944=DIRECTION('',(0.5,0.,-0.866025403784439));
#8945=DIRECTION('',(0.,-1.,0.));
#8946=DIRECTION('',(0.5,0.,-0.866025403784439));
#8947=DIRECTION('center_axis',(-0.866025403784439,0.,0.5));
#8948=DIRECTION('ref_axis',(-0.5,0.,-0.866025403784439));
#8949=DIRECTION('',(-0.5,0.,-0.866025403784439));
#8950=DIRECTION('',(0.,-1.,0.));
#8951=DIRECTION('',(-0.5,0.,-0.866025403784439));
#8952=DIRECTION('center_axis',(-2.40370335797945E-16,0.,1.));
#8953=DIRECTION('ref_axis',(-1.,0.,-2.40370335797945E-16));
#8954=DIRECTION('',(-1.,0.,-2.40370335797945E-16));
#8955=DIRECTION('',(0.,-1.,0.));
#8956=DIRECTION('',(-1.,0.,-2.40370335797945E-16));
#8957=DIRECTION('center_axis',(0.866025403784439,0.,0.5));
#8958=DIRECTION('ref_axis',(-0.5,0.,0.866025403784439));
#8959=DIRECTION('',(-0.5,0.,0.866025403784439));
#8960=DIRECTION('',(-0.5,0.,0.866025403784439));
#8961=DIRECTION('center_axis',(0.,-1.,0.));
#8962=DIRECTION('ref_axis',(0.,0.,-1.));
#8963=DIRECTION('center_axis',(0.,1.,0.));
#8964=DIRECTION('ref_axis',(0.,0.,1.));
#8965=DIRECTION('center_axis',(0.,-1.,0.));
#8966=DIRECTION('ref_axis',(1.,0.,0.));
#8967=DIRECTION('center_axis',(0.,-1.,0.));
#8968=DIRECTION('ref_axis',(1.,0.,0.));
#8969=DIRECTION('center_axis',(0.,-1.,0.));
#8970=DIRECTION('ref_axis',(1.,0.,0.));
#8971=DIRECTION('',(0.707106781186548,0.707106781186547,8.65956056235494E-17));
#8972=DIRECTION('center_axis',(0.,-1.,0.));
#8973=DIRECTION('ref_axis',(1.,0.,0.));
#8974=DIRECTION('',(0.,1.,0.));
#8975=DIRECTION('',(0.,0.,1.));
#8976=DIRECTION('',(1.,0.,0.));
#8977=DIRECTION('',(0.,0.,1.));
#8978=DIRECTION('',(1.,0.,0.));
#8979=DIRECTION('',(0.,0.,1.));
#8980=DIRECTION('',(1.,0.,0.));
#8981=DIRECTION('',(0.,0.,1.));
#8982=DIRECTION('',(1.,0.,0.));
#8983=DIRECTION('',(0.,0.,1.));
#8984=DIRECTION('',(1.,0.,0.));
#8985=DIRECTION('',(0.,0.,1.));
#8986=DIRECTION('',(1.,0.,0.));
#8987=DIRECTION('',(0.,0.,1.));
#8988=DIRECTION('',(1.,0.,0.));
#8989=DIRECTION('',(0.,0.,1.));
#8990=DIRECTION('',(1.,0.,0.));
#8991=DIRECTION('',(0.,-1.,2.22044604925031E-16));
#8992=DIRECTION('',(1.,0.,0.));
#8993=DIRECTION('',(0.,-1.,2.22044604925031E-16));
#8994=DIRECTION('',(1.,0.,0.));
#8995=DIRECTION('',(0.,-1.,2.22044604925031E-16));
#8996=DIRECTION('',(1.,0.,0.));
#8997=DIRECTION('',(0.,-1.,2.22044604925031E-16));
#8998=DIRECTION('',(1.,0.,0.));
#8999=DIRECTION('',(0.,-1.,2.22044604925031E-16));
#9000=DIRECTION('',(1.,0.,0.));
#9001=DIRECTION('',(0.,-1.,2.22044604925031E-16));
#9002=DIRECTION('',(1.,0.,0.));
#9003=DIRECTION('',(0.,0.,1.));
#9004=DIRECTION('',(2.22044604925031E-16,-1.,0.));
#9005=DIRECTION('',(0.,1.,2.22044604925031E-16));
#9006=DIRECTION('',(1.,0.,0.));
#9007=DIRECTION('',(0.,0.,1.));
#9008=DIRECTION('',(1.,0.,0.));
#9009=DIRECTION('',(0.,0.,1.));
#9010=DIRECTION('',(1.,0.,0.));
#9011=DIRECTION('',(0.,1.,2.22044604925031E-16));
#9012=DIRECTION('',(1.,0.,0.));
#9013=DIRECTION('axis',(0.,0.,1.));
#9014=DIRECTION('refdir',(1.,0.,0.));
#9015=DIRECTION('center_axis',(1.,0.,6.12323399573677E-17));
#9016=DIRECTION('ref_axis',(6.12323399573677E-17,0.,-1.));
#9017=DIRECTION('',(1.,0.,6.12323399573677E-17));
#9018=DIRECTION('center_axis',(1.,0.,6.12323399573677E-17));
#9019=DIRECTION('ref_axis',(6.12323399573677E-17,0.,-1.));
#9020=DIRECTION('',(1.,0.,6.12323399573677E-17));
#9021=DIRECTION('center_axis',(0.,-1.,0.));
#9022=DIRECTION('ref_axis',(1.,0.,0.));
#9023=DIRECTION('center_axis',(0.,-1.,0.));
#9024=DIRECTION('ref_axis',(1.,0.,0.));
#9025=DIRECTION('',(0.,1.,0.));
#9026=DIRECTION('',(0.,1.,0.));
#9027=DIRECTION('center_axis',(0.,1.,0.));
#9028=DIRECTION('ref_axis',(1.,0.,0.));
#9029=DIRECTION('center_axis',(0.,0.,1.));
#9030=DIRECTION('ref_axis',(1.,0.,0.));
#9031=DIRECTION('',(0.,0.,1.));
#9032=DIRECTION('center_axis',(0.,0.,1.));
#9033=DIRECTION('ref_axis',(1.,0.,0.));
#9034=DIRECTION('',(0.,0.,1.));
#9035=DIRECTION('center_axis',(0.,1.,0.));
#9036=DIRECTION('ref_axis',(1.,0.,0.));
#9037=DIRECTION('center_axis',(0.,1.,0.));
#9038=DIRECTION('ref_axis',(1.,0.,0.));
#9039=DIRECTION('',(0.,1.,0.));
#9040=DIRECTION('',(0.,1.,0.));
#9041=DIRECTION('center_axis',(0.,-1.,0.));
#9042=DIRECTION('ref_axis',(1.,0.,0.));
#9043=DIRECTION('center_axis',(0.,1.,0.));
#9044=DIRECTION('ref_axis',(1.,0.,0.));
#9045=DIRECTION('center_axis',(0.,1.,0.));
#9046=DIRECTION('ref_axis',(1.,0.,0.));
#9047=DIRECTION('center_axis',(0.,1.,0.));
#9048=DIRECTION('ref_axis',(1.,0.,0.));
#9049=DIRECTION('center_axis',(0.,1.,0.));
#9050=DIRECTION('ref_axis',(0.951056516295154,0.,0.309016994374948));
#9051=DIRECTION('center_axis',(0.,1.,0.));
#9052=DIRECTION('ref_axis',(1.,0.,0.));
#9053=DIRECTION('center_axis',(0.,1.,0.));
#9054=DIRECTION('ref_axis',(0.809016994374947,0.,0.587785252292473));
#9055=DIRECTION('center_axis',(0.,1.,0.));
#9056=DIRECTION('ref_axis',(1.,0.,0.));
#9057=DIRECTION('center_axis',(0.,1.,0.));
#9058=DIRECTION('ref_axis',(0.587785252292473,0.,0.809016994374948));
#9059=DIRECTION('center_axis',(0.,1.,0.));
#9060=DIRECTION('ref_axis',(1.,0.,0.));
#9061=DIRECTION('center_axis',(0.,1.,0.));
#9062=DIRECTION('ref_axis',(0.309016994374947,0.,0.951056516295154));
#9063=DIRECTION('center_axis',(0.,1.,0.));
#9064=DIRECTION('ref_axis',(1.,0.,0.));
#9065=DIRECTION('center_axis',(0.,1.,0.));
#9066=DIRECTION('ref_axis',(-1.83697019872103E-16,0.,1.));
#9067=DIRECTION('center_axis',(0.,1.,0.));
#9068=DIRECTION('ref_axis',(1.,0.,0.));
#9069=DIRECTION('center_axis',(0.,1.,0.));
#9070=DIRECTION('ref_axis',(-0.309016994374948,0.,0.951056516295154));
#9071=DIRECTION('center_axis',(0.,1.,0.));
#9072=DIRECTION('ref_axis',(1.,0.,0.));
#9073=DIRECTION('center_axis',(0.,1.,0.));
#9074=DIRECTION('ref_axis',(-0.587785252292473,0.,0.809016994374947));
#9075=DIRECTION('center_axis',(0.,1.,0.));
#9076=DIRECTION('ref_axis',(1.,0.,0.));
#9077=DIRECTION('center_axis',(0.,1.,0.));
#9078=DIRECTION('ref_axis',(-0.809016994374947,0.,0.587785252292473));
#9079=DIRECTION('center_axis',(0.,1.,0.));
#9080=DIRECTION('ref_axis',(1.,0.,0.));
#9081=DIRECTION('center_axis',(0.,1.,0.));
#9082=DIRECTION('ref_axis',(-0.951056516295154,0.,0.309016994374947));
#9083=DIRECTION('center_axis',(0.,1.,0.));
#9084=DIRECTION('ref_axis',(1.,0.,0.));
#9085=DIRECTION('center_axis',(0.,1.,0.));
#9086=DIRECTION('ref_axis',(-1.,0.,-1.22464679914735E-16));
#9087=DIRECTION('center_axis',(0.,1.,0.));
#9088=DIRECTION('ref_axis',(1.,0.,0.));
#9089=DIRECTION('center_axis',(0.,1.,0.));
#9090=DIRECTION('ref_axis',(-0.951056516295154,0.,-0.309016994374948));
#9091=DIRECTION('center_axis',(0.,1.,0.));
#9092=DIRECTION('ref_axis',(1.,0.,0.));
#9093=DIRECTION('center_axis',(0.,1.,0.));
#9094=DIRECTION('ref_axis',(-0.809016994374947,0.,-0.587785252292473));
#9095=DIRECTION('center_axis',(0.,1.,0.));
#9096=DIRECTION('ref_axis',(1.,0.,0.));
#9097=DIRECTION('center_axis',(0.,1.,0.));
#9098=DIRECTION('ref_axis',(-0.587785252292473,0.,-0.809016994374948));
#9099=DIRECTION('center_axis',(0.,1.,0.));
#9100=DIRECTION('ref_axis',(1.,0.,0.));
#9101=DIRECTION('center_axis',(0.,1.,0.));
#9102=DIRECTION('ref_axis',(-0.309016994374947,0.,-0.951056516295154));
#9103=DIRECTION('center_axis',(0.,1.,0.));
#9104=DIRECTION('ref_axis',(1.,0.,0.));
#9105=DIRECTION('center_axis',(0.,1.,0.));
#9106=DIRECTION('ref_axis',(6.12323399573677E-17,0.,-1.));
#9107=DIRECTION('center_axis',(0.,1.,0.));
#9108=DIRECTION('ref_axis',(1.,0.,0.));
#9109=DIRECTION('center_axis',(0.,1.,0.));
#9110=DIRECTION('ref_axis',(0.309016994374947,0.,-0.951056516295154));
#9111=DIRECTION('center_axis',(0.,1.,0.));
#9112=DIRECTION('ref_axis',(1.,0.,0.));
#9113=DIRECTION('center_axis',(0.,1.,0.));
#9114=DIRECTION('ref_axis',(0.587785252292473,0.,-0.809016994374947));
#9115=DIRECTION('center_axis',(0.,1.,0.));
#9116=DIRECTION('ref_axis',(1.,0.,0.));
#9117=DIRECTION('center_axis',(0.,1.,0.));
#9118=DIRECTION('ref_axis',(0.809016994374947,0.,-0.587785252292473));
#9119=DIRECTION('center_axis',(0.,1.,0.));
#9120=DIRECTION('ref_axis',(1.,0.,0.));
#9121=DIRECTION('center_axis',(0.,1.,0.));
#9122=DIRECTION('ref_axis',(0.951056516295154,0.,-0.309016994374947));
#9123=DIRECTION('center_axis',(0.,1.,0.));
#9124=DIRECTION('ref_axis',(1.,0.,0.));
#9125=DIRECTION('center_axis',(0.,1.,0.));
#9126=DIRECTION('ref_axis',(1.,0.,0.));
#9127=DIRECTION('center_axis',(0.,1.,0.));
#9128=DIRECTION('ref_axis',(1.,0.,0.));
#9129=DIRECTION('center_axis',(0.,-1.,0.));
#9130=DIRECTION('ref_axis',(1.,0.,0.));
#9131=DIRECTION('center_axis',(0.,-1.,0.));
#9132=DIRECTION('ref_axis',(1.,0.,0.));
#9133=DIRECTION('',(0.,1.,0.));
#9134=DIRECTION('center_axis',(0.,1.,0.));
#9135=DIRECTION('ref_axis',(1.,0.,0.));
#9136=DIRECTION('center_axis',(0.,1.,0.));
#9137=DIRECTION('ref_axis',(1.,0.,0.));
#9138=DIRECTION('center_axis',(0.,1.,0.));
#9139=DIRECTION('ref_axis',(1.,0.,0.));
#9140=DIRECTION('center_axis',(0.,-1.,0.));
#9141=DIRECTION('ref_axis',(0.951056516295154,0.,0.309016994374948));
#9142=DIRECTION('center_axis',(0.,1.,0.));
#9143=DIRECTION('ref_axis',(1.,0.,0.));
#9144=DIRECTION('center_axis',(0.,-1.,0.));
#9145=DIRECTION('ref_axis',(1.,0.,0.));
#9146=DIRECTION('center_axis',(0.,1.,0.));
#9147=DIRECTION('ref_axis',(1.,0.,0.));
#9148=DIRECTION('center_axis',(0.,-1.,0.));
#9149=DIRECTION('ref_axis',(0.951056516295154,0.,-0.309016994374947));
#9150=DIRECTION('center_axis',(0.,1.,0.));
#9151=DIRECTION('ref_axis',(1.,0.,0.));
#9152=DIRECTION('center_axis',(0.,-1.,0.));
#9153=DIRECTION('ref_axis',(0.809016994374947,0.,-0.587785252292473));
#9154=DIRECTION('center_axis',(0.,1.,0.));
#9155=DIRECTION('ref_axis',(1.,0.,0.));
#9156=DIRECTION('center_axis',(0.,-1.,0.));
#9157=DIRECTION('ref_axis',(0.587785252292473,0.,-0.809016994374947));
#9158=DIRECTION('center_axis',(0.,1.,0.));
#9159=DIRECTION('ref_axis',(1.,0.,0.));
#9160=DIRECTION('center_axis',(0.,-1.,0.));
#9161=DIRECTION('ref_axis',(0.309016994374947,0.,-0.951056516295154));
#9162=DIRECTION('center_axis',(0.,1.,0.));
#9163=DIRECTION('ref_axis',(1.,0.,0.));
#9164=DIRECTION('center_axis',(0.,-1.,0.));
#9165=DIRECTION('ref_axis',(6.12323399573677E-17,0.,-1.));
#9166=DIRECTION('center_axis',(0.,1.,0.));
#9167=DIRECTION('ref_axis',(1.,0.,0.));
#9168=DIRECTION('center_axis',(0.,-1.,0.));
#9169=DIRECTION('ref_axis',(-0.309016994374947,0.,-0.951056516295154));
#9170=DIRECTION('center_axis',(0.,1.,0.));
#9171=DIRECTION('ref_axis',(1.,0.,0.));
#9172=DIRECTION('center_axis',(0.,-1.,0.));
#9173=DIRECTION('ref_axis',(-0.587785252292473,0.,-0.809016994374948));
#9174=DIRECTION('center_axis',(0.,1.,0.));
#9175=DIRECTION('ref_axis',(1.,0.,0.));
#9176=DIRECTION('center_axis',(0.,-1.,0.));
#9177=DIRECTION('ref_axis',(-0.809016994374947,0.,-0.587785252292473));
#9178=DIRECTION('center_axis',(0.,1.,0.));
#9179=DIRECTION('ref_axis',(1.,0.,0.));
#9180=DIRECTION('center_axis',(0.,-1.,0.));
#9181=DIRECTION('ref_axis',(-0.951056516295154,0.,-0.309016994374948));
#9182=DIRECTION('center_axis',(0.,1.,0.));
#9183=DIRECTION('ref_axis',(1.,0.,0.));
#9184=DIRECTION('center_axis',(0.,-1.,0.));
#9185=DIRECTION('ref_axis',(-1.,0.,-1.22464679914735E-16));
#9186=DIRECTION('center_axis',(0.,1.,0.));
#9187=DIRECTION('ref_axis',(1.,0.,0.));
#9188=DIRECTION('center_axis',(0.,-1.,0.));
#9189=DIRECTION('ref_axis',(-0.951056516295154,0.,0.309016994374947));
#9190=DIRECTION('center_axis',(0.,1.,0.));
#9191=DIRECTION('ref_axis',(1.,0.,0.));
#9192=DIRECTION('center_axis',(0.,-1.,0.));
#9193=DIRECTION('ref_axis',(-0.809016994374947,0.,0.587785252292473));
#9194=DIRECTION('center_axis',(0.,1.,0.));
#9195=DIRECTION('ref_axis',(1.,0.,0.));
#9196=DIRECTION('center_axis',(0.,-1.,0.));
#9197=DIRECTION('ref_axis',(-0.587785252292473,0.,0.809016994374947));
#9198=DIRECTION('center_axis',(0.,1.,0.));
#9199=DIRECTION('ref_axis',(1.,0.,0.));
#9200=DIRECTION('center_axis',(0.,-1.,0.));
#9201=DIRECTION('ref_axis',(-0.309016994374948,0.,0.951056516295154));
#9202=DIRECTION('center_axis',(0.,1.,0.));
#9203=DIRECTION('ref_axis',(1.,0.,0.));
#9204=DIRECTION('center_axis',(0.,-1.,0.));
#9205=DIRECTION('ref_axis',(-1.83697019872103E-16,0.,1.));
#9206=DIRECTION('center_axis',(0.,1.,0.));
#9207=DIRECTION('ref_axis',(1.,0.,0.));
#9208=DIRECTION('center_axis',(0.,-1.,0.));
#9209=DIRECTION('ref_axis',(0.309016994374947,0.,0.951056516295154));
#9210=DIRECTION('center_axis',(0.,1.,0.));
#9211=DIRECTION('ref_axis',(1.,0.,0.));
#9212=DIRECTION('center_axis',(0.,-1.,0.));
#9213=DIRECTION('ref_axis',(0.587785252292473,0.,0.809016994374948));
#9214=DIRECTION('center_axis',(0.,1.,0.));
#9215=DIRECTION('ref_axis',(1.,0.,0.));
#9216=DIRECTION('center_axis',(0.,-1.,0.));
#9217=DIRECTION('ref_axis',(0.809016994374947,0.,0.587785252292473));
#9218=DIRECTION('center_axis',(0.,1.,0.));
#9219=DIRECTION('ref_axis',(1.,0.,0.));
#9220=DIRECTION('center_axis',(0.,1.,0.));
#9221=DIRECTION('ref_axis',(1.,0.,0.));
#9222=DIRECTION('center_axis',(0.,1.,0.));
#9223=DIRECTION('ref_axis',(1.,0.,0.));
#9224=DIRECTION('',(0.,-1.,0.));
#9225=DIRECTION('center_axis',(0.,1.,0.));
#9226=DIRECTION('ref_axis',(1.,0.,0.));
#9227=DIRECTION('center_axis',(0.,1.,0.));
#9228=DIRECTION('ref_axis',(-0.951056516295153,0.,-0.309016994374948));
#9229=DIRECTION('',(0.,-1.,0.));
#9230=DIRECTION('',(0.,1.,0.));
#9231=DIRECTION('center_axis',(0.,1.,0.));
#9232=DIRECTION('ref_axis',(1.,0.,0.));
#9233=DIRECTION('',(0.,-1.,0.));
#9234=DIRECTION('center_axis',(0.,1.,0.));
#9235=DIRECTION('ref_axis',(-0.809016994374947,0.,-0.587785252292473));
#9236=DIRECTION('',(0.,1.,0.));
#9237=DIRECTION('center_axis',(0.,1.,0.));
#9238=DIRECTION('ref_axis',(1.,0.,0.));
#9239=DIRECTION('',(0.,-1.,0.));
#9240=DIRECTION('center_axis',(0.,1.,0.));
#9241=DIRECTION('ref_axis',(-0.587785252292473,0.,-0.809016994374947));
#9242=DIRECTION('',(0.,1.,0.));
#9243=DIRECTION('center_axis',(0.,1.,0.));
#9244=DIRECTION('ref_axis',(1.,0.,0.));
#9245=DIRECTION('',(0.,-1.,0.));
#9246=DIRECTION('center_axis',(0.,1.,0.));
#9247=DIRECTION('ref_axis',(-0.309016994374947,0.,-0.951056516295154));
#9248=DIRECTION('',(0.,1.,0.));
#9249=DIRECTION('center_axis',(0.,1.,0.));
#9250=DIRECTION('ref_axis',(1.,0.,0.));
#9251=DIRECTION('',(0.,-1.,0.));
#9252=DIRECTION('center_axis',(0.,1.,0.));
#9253=DIRECTION('ref_axis',(-1.37927510063224E-16,0.,-1.));
#9254=DIRECTION('',(0.,1.,0.));
#9255=DIRECTION('center_axis',(0.,1.,0.));
#9256=DIRECTION('ref_axis',(1.,0.,0.));
#9257=DIRECTION('',(0.,-1.,0.));
#9258=DIRECTION('center_axis',(0.,1.,0.));
#9259=DIRECTION('ref_axis',(0.309016994374948,0.,-0.951056516295154));
#9260=DIRECTION('',(0.,1.,0.));
#9261=DIRECTION('center_axis',(0.,1.,0.));
#9262=DIRECTION('ref_axis',(1.,0.,0.));
#9263=DIRECTION('',(0.,-1.,0.));
#9264=DIRECTION('center_axis',(0.,1.,0.));
#9265=DIRECTION('ref_axis',(0.587785252292473,0.,-0.809016994374948));
#9266=DIRECTION('',(0.,1.,0.));
#9267=DIRECTION('center_axis',(0.,1.,0.));
#9268=DIRECTION('ref_axis',(1.,0.,0.));
#9269=DIRECTION('',(0.,-1.,0.));
#9270=DIRECTION('center_axis',(0.,1.,0.));
#9271=DIRECTION('ref_axis',(0.809016994374948,0.,-0.587785252292473));
#9272=DIRECTION('',(0.,1.,0.));
#9273=DIRECTION('center_axis',(0.,1.,0.));
#9274=DIRECTION('ref_axis',(1.,0.,0.));
#9275=DIRECTION('',(0.,-1.,0.));
#9276=DIRECTION('center_axis',(0.,1.,0.));
#9277=DIRECTION('ref_axis',(0.951056516295154,0.,-0.309016994374947));
#9278=DIRECTION('',(0.,1.,0.));
#9279=DIRECTION('center_axis',(0.,1.,0.));
#9280=DIRECTION('ref_axis',(1.,0.,0.));
#9281=DIRECTION('',(0.,-1.,0.));
#9282=DIRECTION('center_axis',(0.,1.,0.));
#9283=DIRECTION('ref_axis',(1.,0.,-1.99159850020592E-16));
#9284=DIRECTION('',(0.,1.,0.));
#9285=DIRECTION('center_axis',(0.,1.,0.));
#9286=DIRECTION('ref_axis',(1.,0.,0.));
#9287=DIRECTION('',(0.,-1.,0.));
#9288=DIRECTION('center_axis',(0.,1.,0.));
#9289=DIRECTION('ref_axis',(0.951056516295154,0.,0.309016994374948));
#9290=DIRECTION('',(0.,1.,0.));
#9291=DIRECTION('center_axis',(0.,1.,0.));
#9292=DIRECTION('ref_axis',(1.,0.,0.));
#9293=DIRECTION('',(0.,-1.,0.));
#9294=DIRECTION('center_axis',(0.,1.,0.));
#9295=DIRECTION('ref_axis',(0.809016994374948,0.,0.587785252292473));
#9296=DIRECTION('',(0.,1.,0.));
#9297=DIRECTION('center_axis',(0.,1.,0.));
#9298=DIRECTION('ref_axis',(1.,0.,0.));
#9299=DIRECTION('',(0.,-1.,0.));
#9300=DIRECTION('center_axis',(0.,1.,0.));
#9301=DIRECTION('ref_axis',(0.587785252292473,0.,0.809016994374948));
#9302=DIRECTION('',(0.,1.,0.));
#9303=DIRECTION('center_axis',(0.,1.,0.));
#9304=DIRECTION('ref_axis',(1.,0.,0.));
#9305=DIRECTION('',(0.,-1.,0.));
#9306=DIRECTION('center_axis',(0.,1.,0.));
#9307=DIRECTION('ref_axis',(0.309016994374947,0.,0.951056516295154));
#9308=DIRECTION('',(0.,1.,0.));
#9309=DIRECTION('center_axis',(0.,1.,0.));
#9310=DIRECTION('ref_axis',(1.,0.,0.));
#9311=DIRECTION('',(0.,-1.,0.));
#9312=DIRECTION('center_axis',(0.,1.,0.));
#9313=DIRECTION('ref_axis',(2.6039218997796E-16,0.,1.));
#9314=DIRECTION('',(0.,1.,0.));
#9315=DIRECTION('center_axis',(0.,1.,0.));
#9316=DIRECTION('ref_axis',(1.,0.,0.));
#9317=DIRECTION('',(0.,-1.,0.));
#9318=DIRECTION('center_axis',(0.,1.,0.));
#9319=DIRECTION('ref_axis',(-0.309016994374948,0.,0.951056516295153));
#9320=DIRECTION('',(0.,1.,0.));
#9321=DIRECTION('center_axis',(0.,1.,0.));
#9322=DIRECTION('ref_axis',(1.,0.,0.));
#9323=DIRECTION('',(0.,-1.,0.));
#9324=DIRECTION('center_axis',(0.,1.,0.));
#9325=DIRECTION('ref_axis',(-0.587785252292474,0.,0.809016994374947));
#9326=DIRECTION('',(0.,1.,0.));
#9327=DIRECTION('center_axis',(0.,1.,0.));
#9328=DIRECTION('ref_axis',(1.,0.,0.));
#9329=DIRECTION('',(0.,-1.,0.));
#9330=DIRECTION('center_axis',(0.,1.,0.));
#9331=DIRECTION('ref_axis',(-0.809016994374948,0.,0.587785252292473));
#9332=DIRECTION('',(0.,1.,0.));
#9333=DIRECTION('center_axis',(0.,1.,0.));
#9334=DIRECTION('ref_axis',(1.,0.,0.));
#9335=DIRECTION('',(0.,-1.,0.));
#9336=DIRECTION('center_axis',(0.,1.,0.));
#9337=DIRECTION('ref_axis',(-0.951056516295154,0.,0.309016994374948));
#9338=DIRECTION('',(0.,1.,0.));
#9339=DIRECTION('center_axis',(0.,1.,0.));
#9340=DIRECTION('ref_axis',(1.,0.,0.));
#9341=DIRECTION('',(0.,1.,0.));
#9342=DIRECTION('center_axis',(0.,1.,0.));
#9343=DIRECTION('ref_axis',(-1.,0.,-1.22464679914735E-16));
#9344=DIRECTION('',(0.,-1.,0.));
#9345=DIRECTION('center_axis',(0.,1.,0.));
#9346=DIRECTION('ref_axis',(1.,0.,0.));
#9347=DIRECTION('axis',(0.,0.,1.));
#9348=DIRECTION('refdir',(1.,0.,0.));
#9349=DIRECTION('center_axis',(0.866025403784439,0.,-0.5));
#9350=DIRECTION('ref_axis',(0.5,0.,0.866025403784439));
#9351=DIRECTION('',(-0.5,0.,-0.866025403784439));
#9352=DIRECTION('',(0.,-1.,0.));
#9353=DIRECTION('',(0.5,0.,0.866025403784439));
#9354=DIRECTION('',(0.,-1.,0.));
#9355=DIRECTION('center_axis',(1.60246890531964E-16,0.,-1.));
#9356=DIRECTION('ref_axis',(1.,0.,1.60246890531964E-16));
#9357=DIRECTION('',(-1.,0.,-1.60246890531964E-16));
#9358=DIRECTION('',(0.,-1.,0.));
#9359=DIRECTION('',(1.,0.,1.60246890531964E-16));
#9360=DIRECTION('center_axis',(-0.866025403784439,0.,-0.5));
#9361=DIRECTION('ref_axis',(0.5,0.,-0.866025403784439));
#9362=DIRECTION('',(-0.5,0.,0.866025403784439));
#9363=DIRECTION('',(0.,-1.,0.));
#9364=DIRECTION('',(0.5,0.,-0.866025403784439));
#9365=DIRECTION('center_axis',(-0.866025403784439,0.,0.5));
#9366=DIRECTION('ref_axis',(-0.5,0.,-0.866025403784439));
#9367=DIRECTION('',(0.5,0.,0.866025403784439));
#9368=DIRECTION('',(0.,-1.,0.));
#9369=DIRECTION('',(-0.5,0.,-0.866025403784439));
#9370=DIRECTION('center_axis',(-1.60246890531964E-16,0.,1.));
#9371=DIRECTION('ref_axis',(-1.,0.,-1.60246890531964E-16));
#9372=DIRECTION('',(1.,0.,1.60246890531964E-16));
#9373=DIRECTION('',(0.,-1.,0.));
#9374=DIRECTION('',(-1.,0.,-1.60246890531964E-16));
#9375=DIRECTION('center_axis',(0.866025403784439,0.,0.5));
#9376=DIRECTION('ref_axis',(-0.5,0.,0.866025403784439));
#9377=DIRECTION('',(0.5,0.,-0.866025403784439));
#9378=DIRECTION('',(-0.5,0.,0.866025403784439));
#9379=DIRECTION('center_axis',(0.,1.,0.));
#9380=DIRECTION('ref_axis',(1.,0.,0.));
#9381=DIRECTION('center_axis',(0.,-1.,0.));
#9382=DIRECTION('ref_axis',(0.,0.,-1.));
#9383=DIRECTION('center_axis',(0.,1.,0.));
#9384=DIRECTION('ref_axis',(1.,0.,0.));
#9385=DIRECTION('center_axis',(0.,1.,0.));
#9386=DIRECTION('ref_axis',(1.,0.,0.));
#9387=DIRECTION('center_axis',(0.,1.,0.));
#9388=DIRECTION('ref_axis',(0.,0.,1.));
#9389=DIRECTION('center_axis',(0.,-1.,0.));
#9390=DIRECTION('ref_axis',(1.,0.,0.));
#9391=DIRECTION('center_axis',(0.,-1.,0.));
#9392=DIRECTION('ref_axis',(1.,0.,0.));
#9393=DIRECTION('center_axis',(0.,-1.,0.));
#9394=DIRECTION('ref_axis',(1.,0.,0.));
#9395=DIRECTION('',(0.707106781186547,0.707106781186548,8.65956056235493E-17));
#9396=DIRECTION('center_axis',(0.,-1.,0.));
#9397=DIRECTION('ref_axis',(1.,0.,0.));
#9398=DIRECTION('center_axis',(0.,-1.,0.));
#9399=DIRECTION('ref_axis',(1.,0.,0.));
#9400=DIRECTION('',(0.,1.,0.));
#9401=DIRECTION('center_axis',(0.,1.,0.));
#9402=DIRECTION('ref_axis',(1.,0.,0.));
#9403=DIRECTION('center_axis',(0.,-1.,0.));
#9404=DIRECTION('ref_axis',(1.,0.,0.));
#9405=DIRECTION('',(-0.707106781186547,0.707106781186548,-8.65956056235493E-17));
#9406=DIRECTION('center_axis',(0.,-1.,0.));
#9407=DIRECTION('ref_axis',(0.,0.,-1.));
#9408=DIRECTION('center_axis',(0.,-1.,0.));
#9409=DIRECTION('ref_axis',(1.,0.,0.));
#9410=DIRECTION('center_axis',(0.,1.,0.));
#9411=DIRECTION('ref_axis',(1.,0.,0.));
#9412=DIRECTION('center_axis',(0.,1.,0.));
#9413=DIRECTION('ref_axis',(1.,0.,0.));
#9414=DIRECTION('',(-0.447213595499958,0.894427190999916,-5.47678698264203E-17));
#9415=DIRECTION('center_axis',(0.,-1.,0.));
#9416=DIRECTION('ref_axis',(1.,0.,0.));
#9417=DIRECTION('',(0.,1.,0.));
#9418=DIRECTION('',(0.,0.,1.));
#9419=DIRECTION('',(1.,0.,0.));
#9420=DIRECTION('',(0.,0.,1.));
#9421=DIRECTION('',(1.,0.,0.));
#9422=DIRECTION('',(0.,0.,1.));
#9423=DIRECTION('',(1.,0.,0.));
#9424=DIRECTION('',(0.,0.,1.));
#9425=DIRECTION('',(1.,0.,0.));
#9426=DIRECTION('',(0.,0.,1.));
#9427=DIRECTION('',(1.,0.,0.));
#9428=DIRECTION('',(0.,0.,1.));
#9429=DIRECTION('',(1.,0.,0.));
#9430=DIRECTION('',(0.,0.,1.));
#9431=DIRECTION('',(1.,0.,0.));
#9432=DIRECTION('',(0.,0.,1.));
#9433=DIRECTION('',(2.22044604925031E-16,-1.,0.));
#9434=DIRECTION('',(0.,-1.,2.22044604925031E-16));
#9435=DIRECTION('',(1.,0.,0.));
#9436=DIRECTION('',(0.,-1.,2.22044604925031E-16));
#9437=DIRECTION('',(1.,0.,0.));
#9438=DIRECTION('',(0.,0.,1.));
#9439=DIRECTION('',(1.,0.,0.));
#9440=DIRECTION('',(0.,0.,1.));
#9441=DIRECTION('',(1.,0.,0.));
#9442=DIRECTION('',(0.,0.,1.));
#9443=DIRECTION('',(1.,0.,0.));
#9444=CARTESIAN_POINT('',(0.,0.,0.));
#9445=CARTESIAN_POINT('',(0.,0.,0.));
#9446=CARTESIAN_POINT('',(0.,0.,0.));
#9447=CARTESIAN_POINT('Origin',(6.,1.9,-1.1));
#9448=CARTESIAN_POINT('',(5.775,1.9,-1.));
#9449=CARTESIAN_POINT('Origin',(6.,1.9,-1.));
#9450=CARTESIAN_POINT('',(5.775,1.9,0.));
#9451=CARTESIAN_POINT('',(5.775,1.9,-1.1));
#9452=CARTESIAN_POINT('Origin',(6.,1.9,0.));
#9453=CARTESIAN_POINT('Origin',(0.8,-3.5,-1.1));
#9454=CARTESIAN_POINT('',(0.575,-3.5,-1.));
#9455=CARTESIAN_POINT('Origin',(0.8,-3.5,-1.));
#9456=CARTESIAN_POINT('',(0.575,-3.5,0.));
#9457=CARTESIAN_POINT('',(0.575,-3.5,-1.1));
#9458=CARTESIAN_POINT('Origin',(0.8,-3.5,0.));
#9459=CARTESIAN_POINT('Origin',(2.2,0.,-1.1));
#9460=CARTESIAN_POINT('',(1.99,-2.57175827820944E-17,-1.));
#9461=CARTESIAN_POINT('Origin',(2.2,0.,-1.));
#9462=CARTESIAN_POINT('',(1.99,2.57175827820944E-17,0.));
#9463=CARTESIAN_POINT('',(1.99,-2.57175827820944E-17,-1.1));
#9464=CARTESIAN_POINT('Origin',(2.2,0.,0.));
#9465=CARTESIAN_POINT('Origin',(-1.1,1.90525588832577,-1.1));
#9466=CARTESIAN_POINT('',(-1.31,1.90525588832577,-1.));
#9467=CARTESIAN_POINT('Origin',(-1.1,1.90525588832577,-1.));
#9468=CARTESIAN_POINT('',(-1.31,1.90525588832577,0.));
#9469=CARTESIAN_POINT('',(-1.31,1.90525588832577,-1.1));
#9470=CARTESIAN_POINT('Origin',(-1.1,1.90525588832577,0.));
#9471=CARTESIAN_POINT('Origin',(-1.1,-1.90525588832576,-1.1));
#9472=CARTESIAN_POINT('',(-1.31,-1.90525588832576,-1.));
#9473=CARTESIAN_POINT('Origin',(-1.1,-1.90525588832576,-1.));
#9474=CARTESIAN_POINT('',(-1.31,-1.90525588832576,0.));
#9475=CARTESIAN_POINT('',(-1.31,-1.90525588832576,-1.1));
#9476=CARTESIAN_POINT('Origin',(-1.1,-1.90525588832576,0.));
#9477=CARTESIAN_POINT('Origin',(13.,5.5,-1.));
#9478=CARTESIAN_POINT('',(13.,5.5,-1.));
#9479=CARTESIAN_POINT('',(-4.,5.5,-1.));
#9480=CARTESIAN_POINT('',(13.,5.5,-1.));
#9481=CARTESIAN_POINT('',(-4.,5.5,0.));
#9482=CARTESIAN_POINT('',(-4.,5.5,-1.));
#9483=CARTESIAN_POINT('',(13.,5.5,0.));
#9484=CARTESIAN_POINT('',(13.,5.5,0.));
#9485=CARTESIAN_POINT('',(13.,5.5,-1.));
#9486=CARTESIAN_POINT('Origin',(13.,-4.5,-1.));
#9487=CARTESIAN_POINT('',(13.,-4.5,-1.));
#9488=CARTESIAN_POINT('',(13.,-4.5,-1.));
#9489=CARTESIAN_POINT('',(13.,-4.5,0.));
#9490=CARTESIAN_POINT('',(13.,-4.5,0.));
#9491=CARTESIAN_POINT('',(13.,-4.5,-1.));
#9492=CARTESIAN_POINT('Origin',(-4.,-4.5,-1.));
#9493=CARTESIAN_POINT('',(-4.,-4.5,-1.));
#9494=CARTESIAN_POINT('',(-4.,-4.5,-1.));
#9495=CARTESIAN_POINT('',(-4.,-4.5,0.));
#9496=CARTESIAN_POINT('',(-4.,-4.5,0.));
#9497=CARTESIAN_POINT('',(-4.,-4.5,-1.));
#9498=CARTESIAN_POINT('Origin',(-4.,5.5,-1.));
#9499=CARTESIAN_POINT('',(-4.,5.5,-1.));
#9500=CARTESIAN_POINT('',(-4.,5.5,0.));
#9501=CARTESIAN_POINT('Origin',(4.5,0.5,0.));
#9502=CARTESIAN_POINT('Origin',(4.5,0.5,-1.));
#9503=CARTESIAN_POINT('',(0.,0.,0.));
#9504=CARTESIAN_POINT('Origin',(-2.,5.5,-1.4));
#9505=CARTESIAN_POINT('',(-2.,5.5,-1.4));
#9506=CARTESIAN_POINT('',(-3.,5.5,-1.4));
#9507=CARTESIAN_POINT('',(-2.,5.5,-1.4));
#9508=CARTESIAN_POINT('',(-3.,5.5,-1.));
#9509=CARTESIAN_POINT('',(-3.,5.5,-1.4));
#9510=CARTESIAN_POINT('',(-2.,5.5,-1.));
#9511=CARTESIAN_POINT('',(-2.,5.5,-1.));
#9512=CARTESIAN_POINT('',(-2.,5.5,-1.4));
#9513=CARTESIAN_POINT('Origin',(-2.,-4.5,-1.4));
#9514=CARTESIAN_POINT('',(-2.,-4.5,-1.4));
#9515=CARTESIAN_POINT('',(-2.,-4.5,-1.4));
#9516=CARTESIAN_POINT('',(-2.,-4.5,-1.));
#9517=CARTESIAN_POINT('',(-2.,-4.5,-1.));
#9518=CARTESIAN_POINT('',(-2.,-4.5,-1.4));
#9519=CARTESIAN_POINT('Origin',(-3.,-4.5,-1.4));
#9520=CARTESIAN_POINT('',(-3.,-4.5,-1.4));
#9521=CARTESIAN_POINT('',(-3.,-4.5,-1.4));
#9522=CARTESIAN_POINT('',(-3.,-4.5,-1.));
#9523=CARTESIAN_POINT('',(-3.,-4.5,-1.));
#9524=CARTESIAN_POINT('',(-3.,-4.5,-1.4));
#9525=CARTESIAN_POINT('Origin',(-3.,5.5,-1.4));
#9526=CARTESIAN_POINT('',(-3.,5.5,-1.4));
#9527=CARTESIAN_POINT('',(-3.,5.5,-1.));
#9528=CARTESIAN_POINT('Origin',(-2.5,0.5,-1.));
#9529=CARTESIAN_POINT('Origin',(-2.5,0.5,-1.4));
#9530=CARTESIAN_POINT('',(0.,0.,0.));
#9531=CARTESIAN_POINT('Origin',(12.,5.5,-1.4));
#9532=CARTESIAN_POINT('',(12.,5.5,-1.4));
#9533=CARTESIAN_POINT('',(11.,5.5,-1.4));
#9534=CARTESIAN_POINT('',(12.,5.5,-1.4));
#9535=CARTESIAN_POINT('',(11.,5.5,-1.));
#9536=CARTESIAN_POINT('',(11.,5.5,-1.4));
#9537=CARTESIAN_POINT('',(12.,5.5,-1.));
#9538=CARTESIAN_POINT('',(12.,5.5,-1.));
#9539=CARTESIAN_POINT('',(12.,5.5,-1.4));
#9540=CARTESIAN_POINT('Origin',(12.,-4.5,-1.4));
#9541=CARTESIAN_POINT('',(12.,-4.5,-1.4));
#9542=CARTESIAN_POINT('',(12.,-4.5,-1.4));
#9543=CARTESIAN_POINT('',(12.,-4.5,-1.));
#9544=CARTESIAN_POINT('',(12.,-4.5,-1.));
#9545=CARTESIAN_POINT('',(12.,-4.5,-1.4));
#9546=CARTESIAN_POINT('Origin',(11.,-4.5,-1.4));
#9547=CARTESIAN_POINT('',(11.,-4.5,-1.4));
#9548=CARTESIAN_POINT('',(11.,-4.5,-1.4));
#9549=CARTESIAN_POINT('',(11.,-4.5,-1.));
#9550=CARTESIAN_POINT('',(11.,-4.5,-1.));
#9551=CARTESIAN_POINT('',(11.,-4.5,-1.4));
#9552=CARTESIAN_POINT('Origin',(11.,5.5,-1.4));
#9553=CARTESIAN_POINT('',(11.,5.5,-1.4));
#9554=CARTESIAN_POINT('',(11.,5.5,-1.));
#9555=CARTESIAN_POINT('Origin',(11.5,0.5,-1.));
#9556=CARTESIAN_POINT('Origin',(11.5,0.5,-1.4));
#9557=CARTESIAN_POINT('',(0.,0.,0.));
#9558=CARTESIAN_POINT('Origin',(2.2,0.,-0.1));
#9559=CARTESIAN_POINT('',(1.925,-3.36777869765522E-17,0.));
#9560=CARTESIAN_POINT('Origin',(2.2,0.,0.));
#9561=CARTESIAN_POINT('',(1.925,3.36777869765522E-17,0.8));
#9562=CARTESIAN_POINT('',(1.925,-3.36777869765522E-17,-0.1));
#9563=CARTESIAN_POINT('Origin',(2.2,0.,0.8));
#9564=CARTESIAN_POINT('Origin',(-1.1,1.90525588832577,-0.1));
#9565=CARTESIAN_POINT('',(-1.375,1.90525588832577,0.));
#9566=CARTESIAN_POINT('Origin',(-1.1,1.90525588832577,0.));
#9567=CARTESIAN_POINT('',(-1.375,1.90525588832577,0.8));
#9568=CARTESIAN_POINT('',(-1.375,1.90525588832577,-0.1));
#9569=CARTESIAN_POINT('Origin',(-1.1,1.90525588832577,0.8));
#9570=CARTESIAN_POINT('Origin',(-1.1,-1.90525588832576,-0.1));
#9571=CARTESIAN_POINT('',(-1.375,-1.90525588832576,0.));
#9572=CARTESIAN_POINT('Origin',(-1.1,-1.90525588832576,0.));
#9573=CARTESIAN_POINT('',(-1.375,-1.90525588832576,0.8));
#9574=CARTESIAN_POINT('',(-1.375,-1.90525588832576,-0.1));
#9575=CARTESIAN_POINT('Origin',(-1.1,-1.90525588832576,0.8));
#9576=CARTESIAN_POINT('Origin',(0.,0.,5.05));
#9577=CARTESIAN_POINT('',(-0.7,-8.57252759403147E-17,5.05));
#9578=CARTESIAN_POINT('Origin',(0.,0.,5.05));
#9579=CARTESIAN_POINT('',(-0.5,-6.12323399573677E-17,5.05));
#9580=CARTESIAN_POINT('Origin',(0.,0.,5.05));
#9581=CARTESIAN_POINT('Origin',(0.,0.,4.5));
#9582=CARTESIAN_POINT('',(-0.7,-8.57252759403147E-17,4.5));
#9583=CARTESIAN_POINT('',(-0.7,-8.57252759403147E-17,4.5));
#9584=CARTESIAN_POINT('Origin',(0.,0.,4.5));
#9585=CARTESIAN_POINT('Origin',(0.,0.,4.5));
#9586=CARTESIAN_POINT('',(-0.5,-6.12323399573677E-17,6.8));
#9587=CARTESIAN_POINT('Origin',(0.,0.,6.8));
#9588=CARTESIAN_POINT('',(-0.5,-6.12323399573677E-17,4.5));
#9589=CARTESIAN_POINT('Origin',(0.,0.,6.8));
#9590=CARTESIAN_POINT('Origin',(0.,0.,0.8));
#9591=CARTESIAN_POINT('',(-2.8,-3.42901103761259E-16,0.8));
#9592=CARTESIAN_POINT('Origin',(0.,0.,0.8));
#9593=CARTESIAN_POINT('',(-1.2,-1.46957615897682E-16,0.8));
#9594=CARTESIAN_POINT('Origin',(0.,0.,0.8));
#9595=CARTESIAN_POINT('Origin',(0.,0.,0.));
#9596=CARTESIAN_POINT('',(-2.8,-3.42901103761259E-16,0.));
#9597=CARTESIAN_POINT('',(-2.8,-3.42901103761259E-16,0.));
#9598=CARTESIAN_POINT('Origin',(0.,0.,0.));
#9599=CARTESIAN_POINT('Origin',(0.,0.,0.));
#9600=CARTESIAN_POINT('',(-1.2,-1.46957615897682E-16,4.5));
#9601=CARTESIAN_POINT('Origin',(0.,0.,4.5));
#9602=CARTESIAN_POINT('',(-1.2,-1.46957615897682E-16,0.));
#9603=CARTESIAN_POINT('Origin',(0.,0.,4.5));
#9604=CARTESIAN_POINT('Origin',(0.,0.,0.));
#9605=CARTESIAN_POINT('',(0.,0.,0.));
#9606=CARTESIAN_POINT('Origin',(0.49,0.,6.35));
#9607=CARTESIAN_POINT('',(0.49,0.122167917228706,6.2390946349359));
#9608=CARTESIAN_POINT('',(0.49,0.122167917228706,6.46090536506409));
#9609=CARTESIAN_POINT('',(0.49,0.122167917228706,5.95));
#9610=CARTESIAN_POINT('Origin',(0.49,0.,6.35));
#9611=CARTESIAN_POINT('Origin',(0.49,0.,6.35));
#9612=CARTESIAN_POINT('',(0.49,-0.122167917228706,6.2390946349359));
#9613=CARTESIAN_POINT('Ctrl Pts',(0.49,-0.122167917228706,6.2390946349359));
#9614=CARTESIAN_POINT('Ctrl Pts',(0.490448531679987,-0.120368913626295,
6.23711294069536));
#9615=CARTESIAN_POINT('Ctrl Pts',(0.490895245371684,-0.118534896565231,
6.23518965877367));
#9616=CARTESIAN_POINT('Ctrl Pts',(0.494795015531646,-0.102111993019358,
6.2187667552278));
#9617=CARTESIAN_POINT('Ctrl Pts',(0.498442514607595,-0.0836597150224318,
6.20609154388858));
#9618=CARTESIAN_POINT('Ctrl Pts',(0.50357781976106,-0.0430495960471596,
6.18920409039234));
#9619=CARTESIAN_POINT('Ctrl Pts',(0.505,-0.020880094330741,6.185));
#9620=CARTESIAN_POINT('Ctrl Pts',(0.505,0.020880094330741,6.185));
#9621=CARTESIAN_POINT('Ctrl Pts',(0.50357781976106,0.0430495960471596,6.18920409039234));
#9622=CARTESIAN_POINT('Ctrl Pts',(0.498442514607595,0.0836597150224318,
6.20609154388858));
#9623=CARTESIAN_POINT('Ctrl Pts',(0.494795015531646,0.102111993019358,6.2187667552278));
#9624=CARTESIAN_POINT('Ctrl Pts',(0.490895245371685,0.118534896565231,6.23518965877367));
#9625=CARTESIAN_POINT('Ctrl Pts',(0.490448531679987,0.120368913626295,6.23711294069536));
#9626=CARTESIAN_POINT('Ctrl Pts',(0.49,0.122167917228706,6.2390946349359));
#9627=CARTESIAN_POINT('',(0.49,-0.122167917228706,6.46090536506409));
#9628=CARTESIAN_POINT('Origin',(0.49,0.,6.35));
#9629=CARTESIAN_POINT('',(0.505,4.88772620902458E-17,6.515));
#9630=CARTESIAN_POINT('Ctrl Pts',(0.505,1.2490009027033E-16,6.515));
#9631=CARTESIAN_POINT('Ctrl Pts',(0.505,-0.0208800943307409,6.515));
#9632=CARTESIAN_POINT('Ctrl Pts',(0.50357781976106,-0.0430495960471596,
6.51079590960766));
#9633=CARTESIAN_POINT('Ctrl Pts',(0.498442514607595,-0.0836597150224318,
6.49390845611142));
#9634=CARTESIAN_POINT('Ctrl Pts',(0.494795015531646,-0.102111993019358,
6.4812332447722));
#9635=CARTESIAN_POINT('Ctrl Pts',(0.490895245371684,-0.118534896565231,
6.46481034122633));
#9636=CARTESIAN_POINT('Ctrl Pts',(0.490448531679987,-0.120368913626296,
6.46288705930464));
#9637=CARTESIAN_POINT('Ctrl Pts',(0.49,-0.122167917228706,6.46090536506409));
#9638=CARTESIAN_POINT('',(0.9,-2.02066721859313E-17,6.515));
#9639=CARTESIAN_POINT('',(0.49,-2.02066721859313E-17,6.515));
#9640=CARTESIAN_POINT('',(0.884745726183518,0.165,6.35));
#9641=CARTESIAN_POINT('Ctrl Pts',(0.884745726183518,0.165,6.35));
#9642=CARTESIAN_POINT('Ctrl Pts',(0.884745726183518,0.165,6.32923124059256));
#9643=CARTESIAN_POINT('Ctrl Pts',(0.885552759505264,0.160839719007584,6.30711110492665));
#9644=CARTESIAN_POINT('Ctrl Pts',(0.888448648150043,0.14398647021669,6.26647293736623));
#9645=CARTESIAN_POINT('Ctrl Pts',(0.890493604851638,0.131295993814186,6.24795075602263));
#9646=CARTESIAN_POINT('Ctrl Pts',(0.89431723432394,0.102049819008125,6.21870458121656));
#9647=CARTESIAN_POINT('Ctrl Pts',(0.896347088899543,0.0835273920906821,
6.20601365401642));
#9648=CARTESIAN_POINT('Ctrl Pts',(0.899208271860583,0.0428883760934128,
6.18916007816136));
#9649=CARTESIAN_POINT('Ctrl Pts',(0.9,0.0207679427235068,6.185));
#9650=CARTESIAN_POINT('Ctrl Pts',(0.9,-0.0207679427235068,6.185));
#9651=CARTESIAN_POINT('Ctrl Pts',(0.899208271860583,-0.0428883760934128,
6.18916007816136));
#9652=CARTESIAN_POINT('Ctrl Pts',(0.896347088899543,-0.0835273920906821,
6.20601365401642));
#9653=CARTESIAN_POINT('Ctrl Pts',(0.89431723432394,-0.102049819008125,6.21870458121656));
#9654=CARTESIAN_POINT('Ctrl Pts',(0.890493604851638,-0.131295993814186,
6.24795075602263));
#9655=CARTESIAN_POINT('Ctrl Pts',(0.888448648150043,-0.14398647021669,6.26647293736623));
#9656=CARTESIAN_POINT('Ctrl Pts',(0.885552759505264,-0.160839719007584,
6.30711110492665));
#9657=CARTESIAN_POINT('Ctrl Pts',(0.884745726183518,-0.165,6.32923124059256));
#9658=CARTESIAN_POINT('Ctrl Pts',(0.884745726183518,-0.165,6.37076875940744));
#9659=CARTESIAN_POINT('Ctrl Pts',(0.885552759505264,-0.160839719007584,
6.39288889507334));
#9660=CARTESIAN_POINT('Ctrl Pts',(0.888448648150043,-0.14398647021669,6.43352706263377));
#9661=CARTESIAN_POINT('Ctrl Pts',(0.890493604851638,-0.131295993814186,
6.45204924397737));
#9662=CARTESIAN_POINT('Ctrl Pts',(0.89431723432394,-0.102049819008125,6.48129541878344));
#9663=CARTESIAN_POINT('Ctrl Pts',(0.896347088899543,-0.0835273920906822,
6.49398634598358));
#9664=CARTESIAN_POINT('Ctrl Pts',(0.899208271860583,-0.0428883760934128,
6.51083992183864));
#9665=CARTESIAN_POINT('Ctrl Pts',(0.9,-0.0207679427235068,6.515));
#9666=CARTESIAN_POINT('Ctrl Pts',(0.9,0.,6.515));
#9667=CARTESIAN_POINT('Ctrl Pts',(0.9,-4.16333634234434E-17,6.515));
#9668=CARTESIAN_POINT('Ctrl Pts',(0.9,0.0207679427235068,6.515));
#9669=CARTESIAN_POINT('Ctrl Pts',(0.899208271860583,0.0428883760934128,
6.51083992183864));
#9670=CARTESIAN_POINT('Ctrl Pts',(0.896347088899543,0.0835273920906821,
6.49398634598358));
#9671=CARTESIAN_POINT('Ctrl Pts',(0.89431723432394,0.102049819008125,6.48129541878344));
#9672=CARTESIAN_POINT('Ctrl Pts',(0.890493604851638,0.131295993814186,6.45204924397737));
#9673=CARTESIAN_POINT('Ctrl Pts',(0.888448648150043,0.14398647021669,6.43352706263377));
#9674=CARTESIAN_POINT('Ctrl Pts',(0.885552759505264,0.160839719007584,6.39288889507334));
#9675=CARTESIAN_POINT('Ctrl Pts',(0.884745726183518,0.165,6.37076875940744));
#9676=CARTESIAN_POINT('Ctrl Pts',(0.884745726183518,0.165,6.35));
#9677=CARTESIAN_POINT('Ctrl Pts',(0.49,0.122167917228706,6.46090536506409));
#9678=CARTESIAN_POINT('Ctrl Pts',(0.490448531679987,0.120368913626296,6.46288705930464));
#9679=CARTESIAN_POINT('Ctrl Pts',(0.490895245371684,0.118534896565231,6.46481034122633));
#9680=CARTESIAN_POINT('Ctrl Pts',(0.494795015531646,0.102111993019358,6.4812332447722));
#9681=CARTESIAN_POINT('Ctrl Pts',(0.498442514607595,0.0836597150224318,
6.49390845611142));
#9682=CARTESIAN_POINT('Ctrl Pts',(0.50357781976106,0.0430495960471596,6.51079590960766));
#9683=CARTESIAN_POINT('Ctrl Pts',(0.505,0.0208800943307409,6.515));
#9684=CARTESIAN_POINT('Ctrl Pts',(0.505,-1.11022302462516E-16,6.515));
#9685=CARTESIAN_POINT('Origin',(0.49,0.,6.35));
#9686=CARTESIAN_POINT('',(0.49,-0.122167917228706,5.95));
#9687=CARTESIAN_POINT('Origin',(0.,0.,5.95));
#9688=CARTESIAN_POINT('',(-0.505,-6.18446633569413E-17,6.75));
#9689=CARTESIAN_POINT('Origin',(0.,0.,6.75));
#9690=CARTESIAN_POINT('',(-0.505,-6.18446633569413E-17,5.95));
#9691=CARTESIAN_POINT('',(-0.505,-6.18446633569413E-17,5.95));
#9692=CARTESIAN_POINT('Origin',(0.,0.,5.95));
#9693=CARTESIAN_POINT('Origin',(0.,0.,5.95));
#9694=CARTESIAN_POINT('',(-0.9,-1.10218211923262E-16,6.75));
#9695=CARTESIAN_POINT('Origin',(0.,0.,6.75));
#9696=CARTESIAN_POINT('',(-0.9,-1.10218211923262E-16,5.95));
#9697=CARTESIAN_POINT('',(-0.9,-1.10218211923262E-16,5.95));
#9698=CARTESIAN_POINT('Origin',(0.,0.,5.95));
#9699=CARTESIAN_POINT('Origin',(0.,0.,6.75));
#9700=CARTESIAN_POINT('Origin',(0.,0.,5.95));
#9701=CARTESIAN_POINT('',(0.,0.,0.));
#9702=CARTESIAN_POINT('Origin',(0.8,-3.5,-0.1));
#9703=CARTESIAN_POINT('',(0.635,-3.5,0.));
#9704=CARTESIAN_POINT('Origin',(0.8,-3.5,0.));
#9705=CARTESIAN_POINT('',(0.635,-3.5,1.1));
#9706=CARTESIAN_POINT('',(0.635,-3.5,-0.1));
#9707=CARTESIAN_POINT('Origin',(0.8,-3.5,1.1));
#9708=CARTESIAN_POINT('Origin',(0.8,-3.5,1.1));
#9709=CARTESIAN_POINT('Origin',(0.8,-4.1,6.85));
#9710=CARTESIAN_POINT('',(0.73,-3.99507575177946,6.85));
#9711=CARTESIAN_POINT('Ctrl Pts',(0.73,-3.99507575177946,6.85));
#9712=CARTESIAN_POINT('Ctrl Pts',(0.73,-3.99507575177946,6.85880184230815));
#9713=CARTESIAN_POINT('Ctrl Pts',(0.731761420910135,-3.99533471984804,6.86818235803024));
#9714=CARTESIAN_POINT('Ctrl Pts',(0.738908745654556,-3.99626691094106,6.88542542296838));
#9715=CARTESIAN_POINT('Ctrl Pts',(0.744294025343202,-3.99692632385861,6.89328897470932));
#9716=CARTESIAN_POINT('Ctrl Pts',(0.756710943370877,-3.99816160380442,6.90570589273699));
#9717=CARTESIAN_POINT('Ctrl Pts',(0.764574530564745,-3.99881818552376,6.91109123666712));
#9718=CARTESIAN_POINT('Ctrl Pts',(0.781817716198034,-3.99974388505215,6.91823860827541));
#9719=CARTESIAN_POINT('Ctrl Pts',(0.79119827383024,-4.,6.92));
#9720=CARTESIAN_POINT('Ctrl Pts',(0.80880172616976,-4.,6.92));
#9721=CARTESIAN_POINT('Ctrl Pts',(0.818182283801966,-3.99974388505215,6.91823860827541));
#9722=CARTESIAN_POINT('Ctrl Pts',(0.835425469435255,-3.99881818552376,6.91109123666712));
#9723=CARTESIAN_POINT('Ctrl Pts',(0.843289056629123,-3.99816160380442,6.90570589273699));
#9724=CARTESIAN_POINT('Ctrl Pts',(0.855705974656798,-3.99692632385861,6.89328897470932));
#9725=CARTESIAN_POINT('Ctrl Pts',(0.861091254345444,-3.99626691094106,6.88542542296838));
#9726=CARTESIAN_POINT('Ctrl Pts',(0.868238579089865,-3.99533471984804,6.86818235803024));
#9727=CARTESIAN_POINT('Ctrl Pts',(0.87,-3.99507575177946,6.85880184230815));
#9728=CARTESIAN_POINT('Ctrl Pts',(0.87,-3.99507575177946,6.84119815769185));
#9729=CARTESIAN_POINT('Ctrl Pts',(0.868238579089865,-3.99533471984804,6.83181764196976));
#9730=CARTESIAN_POINT('Ctrl Pts',(0.861091254345444,-3.99626691094106,6.81457457703162));
#9731=CARTESIAN_POINT('Ctrl Pts',(0.855705974656798,-3.99692632385861,6.80671102529068));
#9732=CARTESIAN_POINT('Ctrl Pts',(0.843289056629123,-3.99816160380442,6.79429410726301));
#9733=CARTESIAN_POINT('Ctrl Pts',(0.835425469435254,-3.99881818552376,6.78890876333288));
#9734=CARTESIAN_POINT('Ctrl Pts',(0.818182283801966,-3.99974388505215,6.78176139172459));
#9735=CARTESIAN_POINT('Ctrl Pts',(0.808801726169761,-4.,6.78));
#9736=CARTESIAN_POINT('Ctrl Pts',(0.79119827383024,-4.,6.78));
#9737=CARTESIAN_POINT('Ctrl Pts',(0.781817716198034,-3.99974388505215,6.78176139172459));
#9738=CARTESIAN_POINT('Ctrl Pts',(0.764574530564745,-3.99881818552376,6.78890876333288));
#9739=CARTESIAN_POINT('Ctrl Pts',(0.756710943370877,-3.99816160380442,6.79429410726301));
#9740=CARTESIAN_POINT('Ctrl Pts',(0.744294025343202,-3.99692632385861,6.80671102529068));
#9741=CARTESIAN_POINT('Ctrl Pts',(0.738908745654557,-3.99626691094106,6.81457457703162));
#9742=CARTESIAN_POINT('Ctrl Pts',(0.731761420910136,-3.99533471984804,6.83181764196976));
#9743=CARTESIAN_POINT('Ctrl Pts',(0.73,-3.99507575177946,6.84119815769185));
#9744=CARTESIAN_POINT('Ctrl Pts',(0.73,-3.99507575177946,6.85));
#9745=CARTESIAN_POINT('',(0.73,-3.00492424822054,6.85));
#9746=CARTESIAN_POINT('',(0.73,-4.1,6.85));
#9747=CARTESIAN_POINT('Ctrl Pts',(0.73,-3.00492424822054,6.85));
#9748=CARTESIAN_POINT('Ctrl Pts',(0.73,-3.00492424822054,6.84119815769185));
#9749=CARTESIAN_POINT('Ctrl Pts',(0.731761420910135,-3.00466528015196,6.83181764196976));
#9750=CARTESIAN_POINT('Ctrl Pts',(0.738908745654556,-3.00373308905894,6.81457457703162));
#9751=CARTESIAN_POINT('Ctrl Pts',(0.744294025343202,-3.00307367614139,6.80671102529068));
#9752=CARTESIAN_POINT('Ctrl Pts',(0.756710943370877,-3.00183839619558,6.79429410726301));
#9753=CARTESIAN_POINT('Ctrl Pts',(0.764574530564745,-3.00118181447624,6.78890876333288));
#9754=CARTESIAN_POINT('Ctrl Pts',(0.781817716198034,-3.00025611494785,6.78176139172459));
#9755=CARTESIAN_POINT('Ctrl Pts',(0.79119827383024,-3.,6.78));
#9756=CARTESIAN_POINT('Ctrl Pts',(0.808801726169761,-3.,6.78));
#9757=CARTESIAN_POINT('Ctrl Pts',(0.818182283801966,-3.00025611494785,6.78176139172459));
#9758=CARTESIAN_POINT('Ctrl Pts',(0.835425469435254,-3.00118181447624,6.78890876333288));
#9759=CARTESIAN_POINT('Ctrl Pts',(0.843289056629123,-3.00183839619558,6.79429410726301));
#9760=CARTESIAN_POINT('Ctrl Pts',(0.855705974656798,-3.00307367614139,6.80671102529068));
#9761=CARTESIAN_POINT('Ctrl Pts',(0.861091254345444,-3.00373308905894,6.81457457703162));
#9762=CARTESIAN_POINT('Ctrl Pts',(0.868238579089865,-3.00466528015196,6.83181764196976));
#9763=CARTESIAN_POINT('Ctrl Pts',(0.87,-3.00492424822054,6.84119815769185));
#9764=CARTESIAN_POINT('Ctrl Pts',(0.87,-3.00492424822054,6.85880184230815));
#9765=CARTESIAN_POINT('Ctrl Pts',(0.868238579089865,-3.00466528015196,6.86818235803024));
#9766=CARTESIAN_POINT('Ctrl Pts',(0.861091254345444,-3.00373308905894,6.88542542296838));
#9767=CARTESIAN_POINT('Ctrl Pts',(0.855705974656798,-3.00307367614139,6.89328897470932));
#9768=CARTESIAN_POINT('Ctrl Pts',(0.843289056629123,-3.00183839619558,6.90570589273699));
#9769=CARTESIAN_POINT('Ctrl Pts',(0.835425469435255,-3.00118181447624,6.91109123666712));
#9770=CARTESIAN_POINT('Ctrl Pts',(0.818182283801966,-3.00025611494785,6.91823860827541));
#9771=CARTESIAN_POINT('Ctrl Pts',(0.80880172616976,-3.,6.92));
#9772=CARTESIAN_POINT('Ctrl Pts',(0.79119827383024,-3.,6.92));
#9773=CARTESIAN_POINT('Ctrl Pts',(0.781817716198034,-3.00025611494785,6.91823860827541));
#9774=CARTESIAN_POINT('Ctrl Pts',(0.764574530564745,-3.00118181447624,6.91109123666712));
#9775=CARTESIAN_POINT('Ctrl Pts',(0.756710943370877,-3.00183839619558,6.90570589273699));
#9776=CARTESIAN_POINT('Ctrl Pts',(0.744294025343202,-3.00307367614139,6.89328897470932));
#9777=CARTESIAN_POINT('Ctrl Pts',(0.738908745654556,-3.00373308905894,6.88542542296838));
#9778=CARTESIAN_POINT('Ctrl Pts',(0.731761420910135,-3.00466528015196,6.86818235803024));
#9779=CARTESIAN_POINT('Ctrl Pts',(0.73,-3.00492424822054,6.85880184230815));
#9780=CARTESIAN_POINT('Ctrl Pts',(0.73,-3.00492424822054,6.85));
#9781=CARTESIAN_POINT('Origin',(0.8,-3.5,0.));
#9782=CARTESIAN_POINT('',(0.3,-3.5,7.2));
#9783=CARTESIAN_POINT('Origin',(0.8,-3.5,7.2));
#9784=CARTESIAN_POINT('',(0.3,-3.5,0.));
#9785=CARTESIAN_POINT('',(0.3,-3.5,0.));
#9786=CARTESIAN_POINT('Origin',(0.8,-3.5,0.));
#9787=CARTESIAN_POINT('Origin',(0.8,-3.5,7.2));
#9788=CARTESIAN_POINT('Origin',(0.8,-3.5,0.));
#9789=CARTESIAN_POINT('',(0.,0.,0.));
#9790=CARTESIAN_POINT('Origin',(0.8,2.5,8.05));
#9791=CARTESIAN_POINT('',(3.,2.5,8.11));
#9792=CARTESIAN_POINT('Origin',(3.,2.5,8.05));
#9793=CARTESIAN_POINT('',(0.8,2.5,8.11));
#9794=CARTESIAN_POINT('',(0.8,2.5,8.11));
#9795=CARTESIAN_POINT('',(0.8,2.5,7.99));
#9796=CARTESIAN_POINT('Origin',(0.8,2.5,8.05));
#9797=CARTESIAN_POINT('Origin',(0.8,2.5,8.05));
#9798=CARTESIAN_POINT('Origin',(3.,2.5,8.05));
#9799=CARTESIAN_POINT('Origin',(0.8,2.5,8.05));
#9800=CARTESIAN_POINT('',(0.8,2.5,8.05));
#9801=CARTESIAN_POINT('Origin',(0.8,2.5,8.05));
#9802=CARTESIAN_POINT('',(0.74,2.5,8.05));
#9803=CARTESIAN_POINT('Origin',(0.8,2.5,8.05));
#9804=CARTESIAN_POINT('Origin',(0.8,2.5,8.05));
#9805=CARTESIAN_POINT('Origin',(0.8,0.,8.05));
#9806=CARTESIAN_POINT('',(0.740018061544387,3.68116671391522E-6,8.05003232801258));
#9807=CARTESIAN_POINT('',(0.859999911467134,-6.70801305127644E-14,8.04989692752013));
#9808=CARTESIAN_POINT('Origin',(0.8,0.,8.05));
#9809=CARTESIAN_POINT('',(0.859872085377142,0.000172980010645474,8.04546127555641));
#9810=CARTESIAN_POINT('Ctrl Pts',(0.859872085377143,0.000172980010644996,
8.04546127555642));
#9811=CARTESIAN_POINT('Ctrl Pts',(0.859954613291757,0.00013063375777587,
8.04655234991555));
#9812=CARTESIAN_POINT('Ctrl Pts',(0.860005150486507,8.81606608541971E-5,
8.04764678325301));
#9813=CARTESIAN_POINT('Ctrl Pts',(0.860024122218985,4.56008323849017E-5,
8.0487434141295));
#9814=CARTESIAN_POINT('Ctrl Pts',(0.860030653976549,3.0947954381455E-5,
8.04912097200569));
#9815=CARTESIAN_POINT('Ctrl Pts',(0.860033440268576,1.62917027234746E-5,
8.04949861025168));
#9816=CARTESIAN_POINT('Ctrl Pts',(0.86003250673194,1.63365101006011E-6,
8.0498762810392));
#9817=CARTESIAN_POINT('Ctrl Pts',(0.740037512403726,7.66502084125951E-6,
8.04995576651375));
#9818=CARTESIAN_POINT('Ctrl Pts',(0.740035813633067,2.29745219354216E-5,
8.04957722865058));
#9819=CARTESIAN_POINT('Ctrl Pts',(0.740037570114014,3.82814117523058E-5,
8.04919872536356));
#9820=CARTESIAN_POINT('Ctrl Pts',(0.740042788070948,5.3583348281363E-5,
8.04882030923245));
#9821=CARTESIAN_POINT('Ctrl Pts',(0.740117194774797,0.000271784968983559,
8.04342419397895));
#9822=CARTESIAN_POINT('Ctrl Pts',(0.740890792150363,0.000487598405839051,
8.03808128898406));
#9823=CARTESIAN_POINT('Ctrl Pts',(0.742380657699473,0.000694100304033197,
8.03294245997655));
#9824=CARTESIAN_POINT('Ctrl Pts',(0.742856687791474,0.000760080162185162,
8.03130054185402));
#9825=CARTESIAN_POINT('Ctrl Pts',(0.743406227546339,0.000825107328953121,
8.02967950161156));
#9826=CARTESIAN_POINT('Ctrl Pts',(0.744030943387962,0.000888935459998242,
8.02808458212714));
#9827=CARTESIAN_POINT('Ctrl Pts',(0.744191077600943,0.000905296606698836,
8.02767575436996));
#9828=CARTESIAN_POINT('Ctrl Pts',(0.744356154182508,0.000921578861224115,
8.02726864444978));
#9829=CARTESIAN_POINT('Ctrl Pts',(0.744526114805664,0.000937780810410216,
8.02686330823041));
#9830=CARTESIAN_POINT('Ctrl Pts',(0.746605445104324,0.00113599851057101,
8.02190434852298));
#9831=CARTESIAN_POINT('Ctrl Pts',(0.749384937540555,0.00131981950420992,
8.01727240895181));
#9832=CARTESIAN_POINT('Ctrl Pts',(0.752732134934782,0.00148661196187375,
8.01305741080169));
#9833=CARTESIAN_POINT('Ctrl Pts',(0.754228088577332,0.00156115605210947,
8.01117361337555));
#9834=CARTESIAN_POINT('Ctrl Pts',(0.755838113800148,0.00163228884922257,
8.00937339005261));
#9835=CARTESIAN_POINT('Ctrl Pts',(0.757553006477384,0.00169967923105377,
8.0076667868923));
#9836=CARTESIAN_POINT('Ctrl Pts',(0.761408877509493,0.00185120394428867,
8.00382955452406));
#9837=CARTESIAN_POINT('Ctrl Pts',(0.765741812850314,0.00198196807366009,
8.00051359678304));
#9838=CARTESIAN_POINT('Ctrl Pts',(0.770433984217127,0.00208730979332829,
7.99782013360317));
#9839=CARTESIAN_POINT('Ctrl Pts',(0.772492301163109,0.00213352009337093,
7.99663859088593));
#9840=CARTESIAN_POINT('Ctrl Pts',(0.774620207181123,0.00217481038890225,
7.99557731561769));
#9841=CARTESIAN_POINT('Ctrl Pts',(0.776809296807154,0.00221060862651016,
7.99464766697112));
#9842=CARTESIAN_POINT('Ctrl Pts',(0.778595043257235,0.00223981098303675,
7.99388930753682));
#9843=CARTESIAN_POINT('Ctrl Pts',(0.78041309647326,0.00226521029907004,
7.99322216165319));
#9844=CARTESIAN_POINT('Ctrl Pts',(0.782258231705198,0.00228650951969933,
7.99265080830793));
#9845=CARTESIAN_POINT('Ctrl Pts',(0.787395826455402,0.00234581507204828,
7.99105993198825));
#9846=CARTESIAN_POINT('Ctrl Pts',(0.79274285347778,0.00237362730590223,
7.99020783651138));
#9847=CARTESIAN_POINT('Ctrl Pts',(0.798148945965851,0.00237405188957915,
7.99006491773579));
#9848=CARTESIAN_POINT('Ctrl Pts',(0.798604174158806,0.00237408764228971,
7.99005288304418));
#9849=CARTESIAN_POINT('Ctrl Pts',(0.799059822737112,0.00237392689538011,
7.99004590715478));
#9850=CARTESIAN_POINT('Ctrl Pts',(0.799515801280592,0.00237357083570519,
7.99004398888629));
#9851=CARTESIAN_POINT('Ctrl Pts',(0.804963895587468,0.00236931658577196,
7.99002106915075));
#9852=CARTESIAN_POINT('Ctrl Pts',(0.810387077449856,0.00233753275049762,
7.99071609996183));
#9853=CARTESIAN_POINT('Ctrl Pts',(0.815632511887815,0.00228013906244369,
7.99209871900176));
#9854=CARTESIAN_POINT('Ctrl Pts',(0.817914120610998,0.002255174506911,7.99270011736059));
#9855=CARTESIAN_POINT('Ctrl Pts',(0.820162094552721,0.00222530653908412,
7.99343227420397));
#9856=CARTESIAN_POINT('Ctrl Pts',(0.822363029819604,0.002190429374402,7.99429566671149));
#9857=CARTESIAN_POINT('Ctrl Pts',(0.82639780586693,0.00212649221515163,
7.99587844629669));
#9858=CARTESIAN_POINT('Ctrl Pts',(0.830232389001066,0.0020464716033856,
7.99788444042298));
#9859=CARTESIAN_POINT('Ctrl Pts',(0.833789300856325,0.00194967646796662,
8.00030488653809));
#9860=CARTESIAN_POINT('Ctrl Pts',(0.836638003580475,0.00187215400545616,
8.00224340279105));
#9861=CARTESIAN_POINT('Ctrl Pts',(0.839308650131527,0.00178382077303799,
8.00444829662651));
#9862=CARTESIAN_POINT('Ctrl Pts',(0.841781595032497,0.00168657107783632,
8.00688404387467));
#9863=CARTESIAN_POINT('Ctrl Pts',(0.845652175768119,0.00153435871085521,
8.0106964039365));
#9864=CARTESIAN_POINT('Ctrl Pts',(0.848989336192329,0.00136248698922647,
8.01502206971187));
#9865=CARTESIAN_POINT('Ctrl Pts',(0.851727216776977,0.00117766887422212,
8.01971434681324));
#9866=CARTESIAN_POINT('Ctrl Pts',(0.852925761055746,0.00109676224316106,
8.02176845461684));
#9867=CARTESIAN_POINT('Ctrl Pts',(0.854008975753402,0.00101332668916306,
8.02389331395814));
#9868=CARTESIAN_POINT('Ctrl Pts',(0.854968645475949,0.000927759185469039,
8.02607820491659));
#9869=CARTESIAN_POINT('Ctrl Pts',(0.857147435543468,0.000733490654566433,
8.03103868101274));
#9870=CARTESIAN_POINT('Ctrl Pts',(0.858664126628259,0.000530921213849663,
8.03624259871879));
#9871=CARTESIAN_POINT('Ctrl Pts',(0.85943954321166,0.000324530879757094,
8.04155733118659));
#9872=CARTESIAN_POINT('Ctrl Pts',(0.859628522772982,0.000274230749952153,
8.04285260373016));
#9873=CARTESIAN_POINT('Ctrl Pts',(0.859773244368349,0.00022369573125849,
8.04415453107995));
#9874=CARTESIAN_POINT('Ctrl Pts',(0.859872085377142,0.000172980010645474,
8.04546127555641));
#9875=CARTESIAN_POINT('',(0.74,0.,8.05));
#9876=CARTESIAN_POINT('Origin',(0.8,0.,8.05));
#9877=CARTESIAN_POINT('',(0.8,0.,8.04999999999999));
#9878=CARTESIAN_POINT('Origin',(0.8,-6.66133814775094E-16,8.05));
#9879=CARTESIAN_POINT('Origin',(0.8,-6.66133814775094E-16,8.05));
#9880=CARTESIAN_POINT('Ctrl Pts',(0.799992192036797,0.00474896193479852,
6.79014422086044));
#9881=CARTESIAN_POINT('Ctrl Pts',(0.799967638550529,0.184896450338747,6.80443713908974));
#9882=CARTESIAN_POINT('Ctrl Pts',(0.674670361705441,0.543455008309391,6.8330594352144));
#9883=CARTESIAN_POINT('Ctrl Pts',(0.189034209544693,0.849439608053688,6.87617354971506));
#9884=CARTESIAN_POINT('Ctrl Pts',(-0.287258299249701,0.795379885058583,
6.91224027998794));
#9885=CARTESIAN_POINT('Ctrl Pts',(-0.550325497980241,0.607926215999118,
6.93756224237155));
#9886=CARTESIAN_POINT('Ctrl Pts',(-0.668135787638992,0.468370262290034,
6.95205278987894));
#9887=CARTESIAN_POINT('Ctrl Pts',(-0.797681515793003,0.249601245171223,
6.97219797725517));
#9888=CARTESIAN_POINT('Ctrl Pts',(-0.842241289744138,-0.0491002547813337,
6.99521334099182));
#9889=CARTESIAN_POINT('Ctrl Pts',(-0.732812122296168,-0.403197173369283,
7.02435916833342));
#9890=CARTESIAN_POINT('Ctrl Pts',(-0.524668382980495,-0.664806008100517,
7.0503201318013));
#9891=CARTESIAN_POINT('Ctrl Pts',(-0.184652568425117,-0.828760962866216,
7.07959861118036));
#9892=CARTESIAN_POINT('Ctrl Pts',(0.130453782933179,-0.82870656943649,7.10405631433573));
#9893=CARTESIAN_POINT('Ctrl Pts',(0.364375751582702,-0.746687575144636,
7.12365775087804));
#9894=CARTESIAN_POINT('Ctrl Pts',(0.574616121324387,-0.614810215974657,
7.14328235821488));
#9895=CARTESIAN_POINT('Ctrl Pts',(0.772150732123964,-0.367420603086453,
7.16785616546509));
#9896=CARTESIAN_POINT('Ctrl Pts',(0.856997117769862,0.00408861547259015,
7.19741267271575));
#9897=CARTESIAN_POINT('Ctrl Pts',(0.772201652552023,0.376032772307348,7.22703591400899));
#9898=CARTESIAN_POINT('Ctrl Pts',(0.507351873091063,0.709199534687239,7.26002305113266));
#9899=CARTESIAN_POINT('Ctrl Pts',(0.143736848284574,0.852002078379093,7.28978615651597));
#9900=CARTESIAN_POINT('Ctrl Pts',(-0.234502546384647,0.823108658745492,
7.31961111148852));
#9901=CARTESIAN_POINT('Ctrl Pts',(-0.542883282495364,0.675129422402413,
7.34616719094667));
#9902=CARTESIAN_POINT('Ctrl Pts',(-0.783396359273759,0.37345029211527,7.3761020331664));
#9903=CARTESIAN_POINT('Ctrl Pts',(-0.884489493081995,-0.0661466723839558,
7.41109301032321));
#9904=CARTESIAN_POINT('Ctrl Pts',(-0.709418296017906,-0.569369739308696,
7.45117535759087));
#9905=CARTESIAN_POINT('Ctrl Pts',(-0.19989068769657,-0.889667511851702,
7.49638689971083));
#9906=CARTESIAN_POINT('Ctrl Pts',(0.398973895326053,-0.822339305277361,
7.54171055210185));
#9907=CARTESIAN_POINT('Ctrl Pts',(0.826865587387622,-0.395358142551438,
7.58713932258037));
#9908=CARTESIAN_POINT('Ctrl Pts',(0.894293657405342,0.206666783144423,7.6326658525427));
#9909=CARTESIAN_POINT('Ctrl Pts',(0.607352590357856,0.662764035303079,7.67321405418637));
#9910=CARTESIAN_POINT('Ctrl Pts',(0.194215191945802,0.860916697467946,7.70874703376387));
#9911=CARTESIAN_POINT('Ctrl Pts',(-0.198496552114366,0.86128604965953,7.7392380606388));
#9912=CARTESIAN_POINT('Ctrl Pts',(-0.552965374281963,0.690483866395827,
7.76976084505319));
#9913=CARTESIAN_POINT('Ctrl Pts',(-0.798625493103115,0.382774108679761,
7.80031292414605));
#9914=CARTESIAN_POINT('Ctrl Pts',(-0.886090514398701,-0.00135276288038935,
7.83089169974969));
#9915=CARTESIAN_POINT('Ctrl Pts',(-0.784450923473031,-0.450417071001065,
7.86659566812776));
#9916=CARTESIAN_POINT('Ctrl Pts',(-0.401130832210515,-0.834733160113732,
7.90743505712395));
#9917=CARTESIAN_POINT('Ctrl Pts',(0.206987829997999,-0.903462960885791,
7.95342319362056));
#9918=CARTESIAN_POINT('Ctrl Pts',(0.725081242328631,-0.57760276120548,7.99943459556092));
#9919=CARTESIAN_POINT('Ctrl Pts',(0.859845779758374,-0.192969267412252,
8.03013735189051));
#9920=CARTESIAN_POINT('Ctrl Pts',(0.85987212861708,0.000350822954683268,
8.04547538565828));
#9921=CARTESIAN_POINT('Ctrl Pts',(0.782083895515197,0.00474658906385578,
6.7901433641864));
#9922=CARTESIAN_POINT('Ctrl Pts',(0.782059882823066,0.180926302609037,6.804121478795));
#9923=CARTESIAN_POINT('Ctrl Pts',(0.659555973271399,0.531487716947758,6.8321048287837));
#9924=CARTESIAN_POINT('Ctrl Pts',(0.184633116814794,0.830760271314604,6.87426980269771));
#9925=CARTESIAN_POINT('Ctrl Pts',(-0.281260451809225,0.77788801176931,6.90954769821697));
#9926=CARTESIAN_POINT('Ctrl Pts',(-0.538641971540873,0.594493606073614,
6.93432208193731));
#9927=CARTESIAN_POINT('Ctrl Pts',(-0.653918190481005,0.457939407603894,
6.94850083234196));
#9928=CARTESIAN_POINT('Ctrl Pts',(-0.780687953317182,0.24386073084139,6.96821417260151));
#9929=CARTESIAN_POINT('Ctrl Pts',(-0.824314307227793,-0.0484926765471151,
6.99074018142266));
#9930=CARTESIAN_POINT('Ctrl Pts',(-0.717187592119459,-0.39515858636662,
7.01927419391762));
#9931=CARTESIAN_POINT('Ctrl Pts',(-0.513375485381163,-0.651339249880567,
7.04469559652104));
#9932=CARTESIAN_POINT('Ctrl Pts',(-0.18032688172712,-0.811949801148858,
7.07337464673134));
#9933=CARTESIAN_POINT('Ctrl Pts',(0.128427340685738,-0.811907838078087,
7.09733900644489));
#9934=CARTESIAN_POINT('Ctrl Pts',(0.357695972714028,-0.731523164591556,
7.11655037491275));
#9935=CARTESIAN_POINT('Ctrl Pts',(0.563791009551169,-0.602248940512661,
7.13578788095882));
#9936=CARTESIAN_POINT('Ctrl Pts',(0.75749315843225,-0.359680144541225,7.15988348127248));
#9937=CARTESIAN_POINT('Ctrl Pts',(0.840739127744584,0.00474265771027548,
7.18887631751055));
#9938=CARTESIAN_POINT('Ctrl Pts',(0.757542143832615,0.369752074104698,7.21794685951956));
#9939=CARTESIAN_POINT('Ctrl Pts',(0.497538985691502,0.69685828530355,7.25033241461142));
#9940=CARTESIAN_POINT('Ctrl Pts',(0.14037263865275,0.837164983887327,7.27956858898822));
#9941=CARTESIAN_POINT('Ctrl Pts',(-0.23135335299626,0.808779563585517,7.30887964110316));
#9942=CARTESIAN_POINT('Ctrl Pts',(-0.534553583157228,0.663306227172658,
7.33498883247858));
#9943=CARTESIAN_POINT('Ctrl Pts',(-0.771160823931885,0.366562149115926,
7.36443528633921));
#9944=CARTESIAN_POINT('Ctrl Pts',(-0.870684139974891,-0.066085974814,7.39887368559955));
#9945=CARTESIAN_POINT('Ctrl Pts',(-0.698328687945324,-0.561724009713536,
7.43834986568262));
#9946=CARTESIAN_POINT('Ctrl Pts',(-0.196117757216787,-0.877529134736446,
7.48291619387264));
#9947=CARTESIAN_POINT('Ctrl Pts',(0.394743019079569,-0.811191649286449,
7.52763305566212));
#9948=CARTESIAN_POINT('Ctrl Pts',(0.81736602063245,-0.389604577121731,7.57249504917915));
#9949=CARTESIAN_POINT('Ctrl Pts',(0.884116043254209,0.205474962906694,7.61749685897569));
#9950=CARTESIAN_POINT('Ctrl Pts',(0.600276565017539,0.656805803364734,7.65761681609474));
#9951=CARTESIAN_POINT('Ctrl Pts',(0.191169205453925,0.853065704046926,7.69280415993483));
#9952=CARTESIAN_POINT('Ctrl Pts',(-0.19798749521213,0.853460360938559,7.72301919980889));
#9953=CARTESIAN_POINT('Ctrl Pts',(-0.549503313068882,0.68411551039788,7.75328641528884));
#9954=CARTESIAN_POINT('Ctrl Pts',(-0.793301852382218,0.378787453389241,
7.78360396950921));
#9955=CARTESIAN_POINT('Ctrl Pts',(-0.880186024863404,-0.00265264652523096,
7.81396924276319));
#9956=CARTESIAN_POINT('Ctrl Pts',(-0.779222443771506,-0.448904993517531,
7.84944930171758));
#9957=CARTESIAN_POINT('Ctrl Pts',(-0.398034992400597,-0.831218430880183,
7.89006870656519));
#9958=CARTESIAN_POINT('Ctrl Pts',(0.207454027684503,-0.899761502606193,
7.93585934905774));
#9959=CARTESIAN_POINT('Ctrl Pts',(0.723947436484212,-0.575045194343942,
7.98172266468812));
#9960=CARTESIAN_POINT('Ctrl Pts',(0.858495280337168,-0.191231028022566,
8.01236184878027));
#9961=CARTESIAN_POINT('Ctrl Pts',(0.858521584804765,0.00176336728401826,
8.02767404187196));
#9962=CARTESIAN_POINT('Ctrl Pts',(0.746211861175701,0.00337911061953199,
6.80731739539198));
#9963=CARTESIAN_POINT('Ctrl Pts',(0.746188933644134,0.171597064764558,6.82066382328057));
#9964=CARTESIAN_POINT('Ctrl Pts',(0.629300643905895,0.505942199544543,6.84735079201033));
#9965=CARTESIAN_POINT('Ctrl Pts',(0.176589535284547,0.791165596604293,6.88754110635019));
#9966=CARTESIAN_POINT('Ctrl Pts',(-0.267122090093055,0.740741855173879,
6.92113590965913));
#9967=CARTESIAN_POINT('Ctrl Pts',(-0.512154380788647,0.566142234255932,
6.94472155200791));
#9968=CARTESIAN_POINT('Ctrl Pts',(-0.621881987091332,0.43615820692645,6.95821760793587));
#9969=CARTESIAN_POINT('Ctrl Pts',(-0.74253529346074,0.232406920931183,6.97697939452374));
#9970=CARTESIAN_POINT('Ctrl Pts',(-0.784032142894782,-0.0457619996394047,
6.99841041192963));
#9971=CARTESIAN_POINT('Ctrl Pts',(-0.682117732110117,-0.375558705039205,
7.02555581439515));
#9972=CARTESIAN_POINT('Ctrl Pts',(-0.488256756238947,-0.619222960670186,
7.04973308403748));
#9973=CARTESIAN_POINT('Ctrl Pts',(-0.171488008056215,-0.771983305067387,
7.0770099902553));
#9974=CARTESIAN_POINT('Ctrl Pts',(0.122149257398574,-0.771940192929056,
7.09979855320445));
#9975=CARTESIAN_POINT('Ctrl Pts',(0.340211353718798,-0.695486110106044,
7.11807045248607));
#9976=CARTESIAN_POINT('Ctrl Pts',(0.53623820285835,-0.572527321706746,7.13636752838297));
#9977=CARTESIAN_POINT('Ctrl Pts',(0.720489227996175,-0.341802196164832,
7.15928518411744));
#9978=CARTESIAN_POINT('Ctrl Pts',(0.799693173144715,0.00489118347571509,
7.1868659148334));
#9979=CARTESIAN_POINT('Ctrl Pts',(0.720533952481635,0.35223376988072,7.21452830637497));
#9980=CARTESIAN_POINT('Ctrl Pts',(0.4730649341289,0.663591432522345,7.24535155971625));
#9981=CARTESIAN_POINT('Ctrl Pts',(0.132960879091397,0.79722593466705,7.27319113961288));
#9982=CARTESIAN_POINT('Ctrl Pts',(-0.221169909840595,0.770191731078306,
7.30111344023989));
#9983=CARTESIAN_POINT('Ctrl Pts',(-0.510129926337539,0.631566987709629,
7.32599432900486));
#9984=CARTESIAN_POINT('Ctrl Pts',(-0.735763837282209,0.348621542769495,
7.3540721600674));
#9985=CARTESIAN_POINT('Ctrl Pts',(-0.83074585327453,-0.0641608327867673,
7.3869287659578));
#9986=CARTESIAN_POINT('Ctrl Pts',(-0.666251881204893,-0.537438189822527,
7.42461915123026));
#9987=CARTESIAN_POINT('Ctrl Pts',(-0.186253797849981,-0.839407882375731,
7.46721707138755));
#9988=CARTESIAN_POINT('Ctrl Pts',(0.379235215212093,-0.776034988224205,
7.51001044866301));
#9989=CARTESIAN_POINT('Ctrl Pts',(0.7843241358807,-0.372132898206059,7.55299798483595));
#9990=CARTESIAN_POINT('Ctrl Pts',(0.848523687541135,0.198935849878105,7.59618388556079));
#9991=CARTESIAN_POINT('Ctrl Pts',(0.575836363091698,0.632786382406762,7.63474102091317));
#9992=CARTESIAN_POINT('Ctrl Pts',(0.182120705834638,0.82172473976296,7.66860508915414));
#9993=CARTESIAN_POINT('Ctrl Pts',(-0.192836060916266,0.822151380448873,
7.69771720303896));
#9994=CARTESIAN_POINT('Ctrl Pts',(-0.531935486527566,0.658842663751575,
7.72691217814189));
#9995=CARTESIAN_POINT('Ctrl Pts',(-0.767436874667562,0.363991194653926,
7.75619251137578));
#9996=CARTESIAN_POINT('Ctrl Pts',(-0.851500538204596,-0.00484208671020629,
7.78555379321598));
#9997=CARTESIAN_POINT('Ctrl Pts',(-0.753813471543185,-0.436920652186791,
7.81990555837298));
#9998=CARTESIAN_POINT('Ctrl Pts',(-0.384264491926787,-0.807797014739186,
7.8592962103847));
#9999=CARTESIAN_POINT('Ctrl Pts',(0.204099197055569,-0.874613173770796,
7.90379252019873));
#10000=CARTESIAN_POINT('Ctrl Pts',(0.707183452191518,-0.558568943332804,
7.94845404074619));
#10001=CARTESIAN_POINT('Ctrl Pts',(0.838610010719861,-0.184049422120409,
7.97835344453705));
#10002=CARTESIAN_POINT('Ctrl Pts',(0.838635708308469,0.00449233626619855,
7.99331236500559));
#10003=CARTESIAN_POINT('Ctrl Pts',(0.733118691230247,-0.00121541092765636,
6.86520410690199));
#10004=CARTESIAN_POINT('Ctrl Pts',(0.733096176038643,0.163977229099494,
6.87831050609139));
#10005=CARTESIAN_POINT('Ctrl Pts',(0.61822085349322,0.491745228826158,6.90448596327338));
#10006=CARTESIAN_POINT('Ctrl Pts',(0.175970062539601,0.769921108293996,
6.94373227235256));
#10007=CARTESIAN_POINT('Ctrl Pts',(-0.255552194481174,0.720610916570717,
6.97641400866452));
#10008=CARTESIAN_POINT('Ctrl Pts',(-0.493113212192604,0.551270519052718,
6.99928612393978));
#10009=CARTESIAN_POINT('Ctrl Pts',(-0.599352677367421,0.425413827161342,
7.01235409532875));
#10010=CARTESIAN_POINT('Ctrl Pts',(-0.716053322126291,0.228307160798129,
7.0305039837357));
#10011=CARTESIAN_POINT('Ctrl Pts',(-0.755987795799746,-0.0402317376255194,
7.05119646804638));
#10012=CARTESIAN_POINT('Ctrl Pts',(-0.657812414621087,-0.357757242991282,
7.07733373637638));
#10013=CARTESIAN_POINT('Ctrl Pts',(-0.471441715442261,-0.591889140959248,
7.10057459246807));
#10014=CARTESIAN_POINT('Ctrl Pts',(-0.167720266372115,-0.738248710573425,
7.12672490984441));
#10015=CARTESIAN_POINT('Ctrl Pts',(0.113172505182452,-0.73814555008345,
7.14852996458262));
#10016=CARTESIAN_POINT('Ctrl Pts',(0.32139189594574,-0.665125967717377,
7.16597855239755));
#10017=CARTESIAN_POINT('Ctrl Pts',(0.508368992958891,-0.547828363309776,
7.18343278966605));
#10018=CARTESIAN_POINT('Ctrl Pts',(0.68379727163952,-0.328042392259005,
7.20526336568707));
#10019=CARTESIAN_POINT('Ctrl Pts',(0.758995968879483,0.00147100263930197,
7.23147983992185));
#10020=CARTESIAN_POINT('Ctrl Pts',(0.683845346105746,0.330894269024558,
7.25771830557115));
#10021=CARTESIAN_POINT('Ctrl Pts',(0.4494984993554,0.625611121189165,7.28690416485887));
#10022=CARTESIAN_POINT('Ctrl Pts',(0.128190915608229,0.751732271497407,
7.3132032011683));
#10023=CARTESIAN_POINT('Ctrl Pts',(-0.205740395995592,0.726211680022978,
7.33953609531371));
#10024=CARTESIAN_POINT('Ctrl Pts',(-0.47784093637727,0.595622453011025,
7.3629701633916));
#10025=CARTESIAN_POINT('Ctrl Pts',(-0.689925933091511,0.329571628023445,
7.38936942831608));
#10026=CARTESIAN_POINT('Ctrl Pts',(-0.779030370279855,-0.057949305094791,
7.42021638986164));
#10027=CARTESIAN_POINT('Ctrl Pts',(-0.624727627139914,-0.501449572002762,
7.4555452585764));
#10028=CARTESIAN_POINT('Ctrl Pts',(-0.175673176115022,-0.783757181614016,
7.4953950638941));
#10029=CARTESIAN_POINT('Ctrl Pts',(0.352351719308904,-0.724451702416669,
7.5353596505547));
#10030=CARTESIAN_POINT('Ctrl Pts',(0.729970142788671,-0.347752667481679,
7.57544876714829));
#10031=CARTESIAN_POINT('Ctrl Pts',(0.789657111879439,0.1840317456448,7.6156657596193));
#10032=CARTESIAN_POINT('Ctrl Pts',(0.535913030225253,0.58759892475464,7.65154038131291));
#10033=CARTESIAN_POINT('Ctrl Pts',(0.169902356678922,0.763219405476266,
7.68302342417015));
#10034=CARTESIAN_POINT('Ctrl Pts',(-0.178501350955049,0.763599585157561,
7.71007496388204));
#10035=CARTESIAN_POINT('Ctrl Pts',(-0.49348507045862,0.611896218217824,
7.73719675089236));
#10036=CARTESIAN_POINT('Ctrl Pts',(-0.712165255112946,0.338087476205076,
7.76438731081332));
#10037=CARTESIAN_POINT('Ctrl Pts',(-0.790218533611398,-0.00437348680934723,
7.79165189591018));
#10038=CARTESIAN_POINT('Ctrl Pts',(-0.699522824014373,-0.405524976731812,
7.82354572726495));
#10039=CARTESIAN_POINT('Ctrl Pts',(-0.356416098090345,-0.749880696062379,
7.86012337962793));
#10040=CARTESIAN_POINT('Ctrl Pts',(0.189993874214275,-0.811999190746788,
7.90144794605881));
#10041=CARTESIAN_POINT('Ctrl Pts',(0.657467882103646,-0.518362744790317,
7.94295065081735));
#10042=CARTESIAN_POINT('Ctrl Pts',(0.779720660519966,-0.170272821142141,
7.97074475069534));
#10043=CARTESIAN_POINT('Ctrl Pts',(0.779744575002708,0.00518639006840643,
7.98466570066648));
#10044=CARTESIAN_POINT('Ctrl Pts',(0.770161787666388,-0.0049051884182797,
6.91177358097206));
#10045=CARTESIAN_POINT('Ctrl Pts',(0.77013815979716,0.168451102057769,6.92552768493576));
#10046=CARTESIAN_POINT('Ctrl Pts',(0.649534215561946,0.512222733391276,
6.95298053601555));
#10047=CARTESIAN_POINT('Ctrl Pts',(0.187168277555439,0.802638877493012,
6.99399073281223));
#10048=CARTESIAN_POINT('Ctrl Pts',(-0.262198140354615,0.751064960128479,
7.02802547805165));
#10049=CARTESIAN_POINT('Ctrl Pts',(-0.508913103682435,0.575130647460083,
7.05178092432448));
#10050=CARTESIAN_POINT('Ctrl Pts',(-0.619111082011442,0.444578654305825,
7.06533603148814));
#10051=CARTESIAN_POINT('Ctrl Pts',(-0.740044687677081,0.240300892811425,
7.08414438574734));
#10052=CARTESIAN_POINT('Ctrl Pts',(-0.781206914566788,-0.0373853933734546,
7.1055381456328));
#10053=CARTESIAN_POINT('Ctrl Pts',(-0.679897669421572,-0.364897169169454,
7.13249836635836));
#10054=CARTESIAN_POINT('Ctrl Pts',(-0.488024517524781,-0.605802178567223,
7.15641268103637));
#10055=CARTESIAN_POINT('Ctrl Pts',(-0.176195068872705,-0.755957282246966,
7.18325651241199));
#10056=CARTESIAN_POINT('Ctrl Pts',(0.111348212069435,-0.755759824660184,
7.20557366213014));
#10057=CARTESIAN_POINT('Ctrl Pts',(0.324079866150574,-0.681141300007829,
7.22340028977131));
#10058=CARTESIAN_POINT('Ctrl Pts',(0.514846340621651,-0.561445486392157,
7.24120776275288));
#10059=CARTESIAN_POINT('Ctrl Pts',(0.693392023322827,-0.337618657943588,
7.26343091101724));
#10060=CARTESIAN_POINT('Ctrl Pts',(0.769635059289149,-0.00303104269807223,
7.29004601098107));
#10061=CARTESIAN_POINT('Ctrl Pts',(0.693444862893658,0.330499664199637,
7.31661153187426));
#10062=CARTESIAN_POINT('Ctrl Pts',(0.456735603111685,0.627969916924075,
7.34607308215436));
#10063=CARTESIAN_POINT('Ctrl Pts',(0.133325789120308,0.754719670744551,
7.37253732117947));
#10064=CARTESIAN_POINT('Ctrl Pts',(-0.201749074907764,0.72905336280371,
7.39895899203418));
#10065=CARTESIAN_POINT('Ctrl Pts',(-0.474093090444533,0.598239697877912,
7.42241416461049));
#10066=CARTESIAN_POINT('Ctrl Pts',(-0.685720778229502,0.332588035449833,
7.4487655384973));
#10067=CARTESIAN_POINT('Ctrl Pts',(-0.774286915001198,-0.0531887270732548,
7.47946804042779));
#10068=CARTESIAN_POINT('Ctrl Pts',(-0.620932470247468,-0.492950794309791,
7.51450072760456));
#10069=CARTESIAN_POINT('Ctrl Pts',(-0.177226274555884,-0.771445224212861,
7.55385224805798));
#10070=CARTESIAN_POINT('Ctrl Pts',(0.342041485084231,-0.712747358770181,
7.59315236551947));
#10071=CARTESIAN_POINT('Ctrl Pts',(0.711641525266257,-0.3435411547766,7.63240925035107));
#10072=CARTESIAN_POINT('Ctrl Pts',(0.769499498225703,0.175244317707386,
7.67163866408723));
#10073=CARTESIAN_POINT('Ctrl Pts',(0.522731088231096,0.567170601537302,
7.70648697733878));
#10074=CARTESIAN_POINT('Ctrl Pts',(0.168219094722662,0.737140101731971,
7.7369745868455));
#10075=CARTESIAN_POINT('Ctrl Pts',(-0.16835708474472,0.737418193432977,
7.76310610272568));
#10076=CARTESIAN_POINT('Ctrl Pts',(-0.471829280061021,0.591148177243926,
7.78923716628898));
#10077=CARTESIAN_POINT('Ctrl Pts',(-0.68198399086596,0.327873199664767,
7.81537513043843));
#10078=CARTESIAN_POINT('Ctrl Pts',(-0.756748500370122,-0.000565030967214881,
7.84151856236785));
#10079=CARTESIAN_POINT('Ctrl Pts',(-0.669865274993425,-0.38439027917607,
7.87203298976409));
#10080=CARTESIAN_POINT('Ctrl Pts',(-0.342313195892621,-0.712763775423981,
7.90692835262793));
#10081=CARTESIAN_POINT('Ctrl Pts',(0.177398463143254,-0.7716047406813,7.94622450426568));
#10082=CARTESIAN_POINT('Ctrl Pts',(0.620527880128547,-0.492889698198811,
7.98557967631099));
#10083=CARTESIAN_POINT('Ctrl Pts',(0.735934674957884,-0.163847720445079,
8.01184392471022));
#10084=CARTESIAN_POINT('Ctrl Pts',(0.735957278350781,0.00199209850848452,
8.02500167121408));
#10085=CARTESIAN_POINT('Ctrl Pts',(0.829769160098015,-0.00488434981852912,
6.91161333010028));
#10086=CARTESIAN_POINT('Ctrl Pts',(0.829743731513962,0.18168367969413,6.92641565464919));
#10087=CARTESIAN_POINT('Ctrl Pts',(0.699843619304575,0.552076534387807,
6.95599547018192));
#10088=CARTESIAN_POINT('Ctrl Pts',(0.201807308649101,0.864839644355192,
7.00016592964866));
#10089=CARTESIAN_POINT('Ctrl Pts',(-0.282182757851473,0.809306837023904,
7.03682727121008));
#10090=CARTESIAN_POINT('Ctrl Pts',(-0.547830385030607,0.619853772524046,
7.06240625604372));
#10091=CARTESIAN_POINT('Ctrl Pts',(-0.666466802209058,0.479305181004825,
7.07699970635685));
#10092=CARTESIAN_POINT('Ctrl Pts',(-0.796644113642904,0.259407192366027,
7.09724627700515));
#10093=CARTESIAN_POINT('Ctrl Pts',(-0.840912181483199,-0.039422086776628,
7.12027012001651));
#10094=CARTESIAN_POINT('Ctrl Pts',(-0.731934331083525,-0.39168152176215,
7.14926800599663));
#10095=CARTESIAN_POINT('Ctrl Pts',(-0.525629581163318,-0.650666172634783,
7.17498018991238));
#10096=CARTESIAN_POINT('Ctrl Pts',(-0.190594423194871,-0.811959054684044,
7.20382069278616));
#10097=CARTESIAN_POINT('Ctrl Pts',(0.118112171533783,-0.811717843255708,
7.22778228750397));
#10098=CARTESIAN_POINT('Ctrl Pts',(0.34634335321456,-0.731654669484967,
7.24690838696606));
#10099=CARTESIAN_POINT('Ctrl Pts',(0.550917836533123,-0.603286916074073,
7.26600558166793));
#10100=CARTESIAN_POINT('Ctrl Pts',(0.742230550690213,-0.363395535342033,
7.28982294732455));
#10101=CARTESIAN_POINT('Ctrl Pts',(0.823803964770561,-0.00519553417755166,
7.31831706475512));
#10102=CARTESIAN_POINT('Ctrl Pts',(0.742286337798943,0.351438553015085,
7.34672450759284));
#10103=CARTESIAN_POINT('Ctrl Pts',(0.489421995978955,0.6691072759963,7.37819256480912));
#10104=CARTESIAN_POINT('Ctrl Pts',(0.144523960155876,0.804171605789853,
7.40641314354085));
#10105=CARTESIAN_POINT('Ctrl Pts',(-0.212256980349852,0.77681213732754,
7.43454828405317));
#10106=CARTESIAN_POINT('Ctrl Pts',(-0.501871263134857,0.637644584928468,
7.45949448325541));
#10107=CARTESIAN_POINT('Ctrl Pts',(-0.726514202805803,0.355546311452734,
7.4874740822851));
#10108=CARTESIAN_POINT('Ctrl Pts',(-0.820312452345266,-0.0533892841775268,
7.52001935409191));
#10109=CARTESIAN_POINT('Ctrl Pts',(-0.657900019665717,-0.518447994161681,
7.55707673798875));
#10110=CARTESIAN_POINT('Ctrl Pts',(-0.189795967929553,-0.8119193538092,
7.59858280456595));
#10111=CARTESIAN_POINT('Ctrl Pts',(0.35616630218894,-0.749919823012872,
7.63990940642612));
#10112=CARTESIAN_POINT('Ctrl Pts',(0.743338323366643,-0.362709574793551,
7.68106196817871));
#10113=CARTESIAN_POINT('Ctrl Pts',(0.80346227090447,0.17923740027597,7.72204264617022));
#10114=CARTESIAN_POINT('Ctrl Pts',(0.54632793895988,0.587079715364954,7.75832537027638));
#10115=CARTESIAN_POINT('Ctrl Pts',(0.17836408415985,0.763367126788049,7.78996864240415));
#10116=CARTESIAN_POINT('Ctrl Pts',(-0.170075123139509,0.763558723590948,
7.8170221887093));
#10117=CARTESIAN_POINT('Ctrl Pts',(-0.483417494252776,0.612419263894165,
7.84400997409509));
#10118=CARTESIAN_POINT('Ctrl Pts',(-0.699782787807372,0.341192770179666,
7.87093148920761));
#10119=CARTESIAN_POINT('Ctrl Pts',(-0.776490880144409,0.00376884031652594,
7.8977917364649));
#10120=CARTESIAN_POINT('Ctrl Pts',(-0.687344347841935,-0.389454218058659,
7.9290563908098));
#10121=CARTESIAN_POINT('Ctrl Pts',(-0.352645458615756,-0.724542442309527,
7.96469323566261));
#10122=CARTESIAN_POINT('Ctrl Pts',(0.175896300401543,-0.78400788229888,
8.00465601571697));
#10123=CARTESIAN_POINT('Ctrl Pts',(0.62441514988287,-0.501460617098908,
8.04451206072658));
#10124=CARTESIAN_POINT('Ctrl Pts',(0.740592930009457,-0.169640666497113,
8.07099633783989));
#10125=CARTESIAN_POINT('Ctrl Pts',(0.740615682275994,-0.00270857004267862,
8.08424074574123));
#10126=CARTESIAN_POINT('Ctrl Pts',(0.867052181645218,-0.00120175871753932,
6.86526211624204));
#10127=CARTESIAN_POINT('Ctrl Pts',(0.867025620419448,0.193676396638986,
6.88072376693651));
#10128=CARTESIAN_POINT('Ctrl Pts',(0.731274983219511,0.581263904795406,
6.91167582009283));
#10129=CARTESIAN_POINT('Ctrl Pts',(0.208889229873121,0.909653700476453,
6.9580206776033));
#10130=CARTESIAN_POINT('Ctrl Pts',(-0.300406904913673,0.85146343699967,
6.9965998706139));
#10131=CARTESIAN_POINT('Ctrl Pts',(-0.58050096341849,0.651757693532619,
7.0235675335524));
#10132=CARTESIAN_POINT('Ctrl Pts',(-0.705698371138862,0.503443865012817,
7.03896792854912));
#10133=CARTESIAN_POINT('Ctrl Pts',(-0.843167221724989,0.27124909392191,
7.06034804595424));
#10134=CARTESIAN_POINT('Ctrl Pts',(-0.89008391300503,-0.0447685823858592,
7.08469890727413));
#10135=CARTESIAN_POINT('Ctrl Pts',(-0.774684852554919,-0.417890972125979,
7.11541335647561));
#10136=CARTESIAN_POINT('Ctrl Pts',(-0.555918291315305,-0.692620058527589,
7.14268741589426));
#10137=CARTESIAN_POINT('Ctrl Pts',(-0.200074101514066,-0.864003221456998,
7.17332192920839));
#10138=CARTESIAN_POINT('Ctrl Pts',(0.128324923138355,-0.863804881646564,
7.19881425454244));
#10139=CARTESIAN_POINT('Ctrl Pts',(0.371357425002296,-0.77855956076303,
7.21918064418244));
#10140=CARTESIAN_POINT('Ctrl Pts',(0.589346067791464,-0.641787738018295,
7.23953018657742));
#10141=CARTESIAN_POINT('Ctrl Pts',(0.793440636024401,-0.385946008896802,
7.26493567059373));
#10142=CARTESIAN_POINT('Ctrl Pts',(0.880610663516279,-0.00342731245940255,
7.29536655472608));
#10143=CARTESIAN_POINT('Ctrl Pts',(0.793503503400377,0.377874926448799,
7.32573878007044));
#10144=CARTESIAN_POINT('Ctrl Pts',(0.522907380896809,0.717918064055114,
7.35942130926836));
#10145=CARTESIAN_POINT('Ctrl Pts',(0.153358738280526,0.862712152253253,
7.38966141681963));
#10146=CARTESIAN_POINT('Ctrl Pts',(-0.229296456950172,0.83338998728552,
7.41983724018969));
#10147=CARTESIAN_POINT('Ctrl Pts',(-0.540142076806848,0.684056763209437,
7.44661190552654));
#10148=CARTESIAN_POINT('Ctrl Pts',(-0.781447811125426,0.381086249052736,
7.47666399795968));
#10149=CARTESIAN_POINT('Ctrl Pts',(-0.882294636975832,-0.0584199370281204,
7.51164340198535));
#10150=CARTESIAN_POINT('Ctrl Pts',(-0.70767939754827,-0.558645777936402,
7.55150198975409));
#10151=CARTESIAN_POINT('Ctrl Pts',(-0.203895641922302,-0.874560559164748,
7.59617469651437));
#10152=CARTESIAN_POINT('Ctrl Pts',(0.383996736306925,-0.807839822902091,
7.64067503958532));
#10153=CARTESIAN_POINT('Ctrl Pts',(0.801025471050119,-0.390801899647342,
7.6849987482111));
#10154=CARTESIAN_POINT('Ctrl Pts',(0.865780475559091,0.192944577746062,
7.72913998434886));
#10155=CARTESIAN_POINT('Ctrl Pts',(0.588848361386401,0.632155121475723,
7.76821325076472));
#10156=CARTESIAN_POINT('Ctrl Pts',(0.192692163630185,0.821932819753422,
7.80227997108));
#10157=CARTESIAN_POINT('Ctrl Pts',(-0.182308387523879,0.822124958515745,
7.83139543007317));
#10158=CARTESIAN_POINT('Ctrl Pts',(-0.51937325729508,0.659521736920761,
7.86042625847278));
#10159=CARTESIAN_POINT('Ctrl Pts',(-0.751984131238383,0.367894174259561,
7.88937101849458));
#10160=CARTESIAN_POINT('Ctrl Pts',(-0.834378810498797,0.00534130500814561,
7.91823005194813));
#10161=CARTESIAN_POINT('Ctrl Pts',(-0.738628119598523,-0.416845576119052,
7.95179753903771));
#10162=CARTESIAN_POINT('Ctrl Pts',(-0.37957617275833,-0.776169891700485,
7.99001669480089));
#10163=CARTESIAN_POINT('Ctrl Pts',(0.18648963195138,-0.839684907683195,
8.03281502748034));
#10164=CARTESIAN_POINT('Ctrl Pts',(0.665920196130032,-0.537487668578003,
8.07542274768869));
#10165=CARTESIAN_POINT('Ctrl Pts',(0.789769227401029,-0.183278618129617,
8.10368855968049));
#10166=CARTESIAN_POINT('Ctrl Pts',(0.789793474622567,-0.00537812113452141,
8.11780320149054));
#10167=CARTESIAN_POINT('Ctrl Pts',(0.853661640305302,0.00339334784518846,
6.80732253543625));
#10168=CARTESIAN_POINT('Ctrl Pts',(0.853635468008913,0.19541795114282,6.82255778504901));
#10169=CARTESIAN_POINT('Ctrl Pts',(0.719986974510146,0.577745947714341,
6.85307843059456));
#10170=CARTESIAN_POINT('Ctrl Pts',(0.202996091663939,0.9032416170388,6.89896358845432));
#10171=CARTESIAN_POINT('Ctrl Pts',(-0.303109174735908,0.845693094909515,
6.93729140028491));
#10172=CARTESIAN_POINT('Ctrl Pts',(-0.582255539424857,0.646737893808958,
6.9641625146133));
#10173=CARTESIAN_POINT('Ctrl Pts',(-0.707187570039253,0.498743335043288,
6.97952935315777));
#10174=CARTESIAN_POINT('Ctrl Pts',(-0.844496668315667,0.266850006910183,
7.00088222244567));
#10175=CARTESIAN_POINT('Ctrl Pts',(-0.891594037992852,-0.0494074690447157,
7.02524936934462));
#10176=CARTESIAN_POINT('Ctrl Pts',(-0.775864913170373,-0.423790227055181,
7.05606566088994));
#10177=CARTESIAN_POINT('Ctrl Pts',(-0.556014141834938,-0.700023509989886,
7.08348029571907));
#10178=CARTESIAN_POINT('Ctrl Pts',(-0.197442128244194,-0.872850275371536,
7.11435377694941));
#10179=CARTESIAN_POINT('Ctrl Pts',(0.134307910883221,-0.872732581079474,
7.14010240054951));
#10180=CARTESIAN_POINT('Ctrl Pts',(0.380290026930844,-0.786472573424526,
7.16071470827779));
#10181=CARTESIAN_POINT('Ctrl Pts',(0.601188873497654,-0.647894974478719,
7.18133439191931));
#10182=CARTESIAN_POINT('Ctrl Pts',(0.80843467014646,-0.388244947436199,
7.20712128927313));
#10183=CARTESIAN_POINT('Ctrl Pts',(0.897241113296386,0.00096693004960254,
7.23808404606463));
#10184=CARTESIAN_POINT('Ctrl Pts',(0.808491004798083,0.389917959096619,
7.26906263331152));
#10185=CARTESIAN_POINT('Ctrl Pts',(0.531942258526264,0.73763892882448,7.30349537884369));
#10186=CARTESIAN_POINT('Ctrl Pts',(0.153146136882341,0.886248501617647,
7.33449654477937));
#10187=CARTESIAN_POINT('Ctrl Pts',(-0.240065070170912,0.856166302038153,
7.36550226255206));
#10188=CARTESIAN_POINT('Ctrl Pts',(-0.560108122366354,0.702506159088164,
7.39306447981344));
#10189=CARTESIAN_POINT('Ctrl Pts',(-0.809177049333453,0.389950400765561,
7.42407264103054));
#10190=CARTESIAN_POINT('Ctrl Pts',(-0.913577971917155,-0.0645250182065023,
7.46024471429976));
#10191=CARTESIAN_POINT('Ctrl Pts',(-0.732789529640382,-0.583312567393491,
7.50157210267981));
#10192=CARTESIAN_POINT('Ctrl Pts',(-0.20889138072868,-0.912238145067271,
7.54804130641669));
#10193=CARTESIAN_POINT('Ctrl Pts',(0.404620472690996,-0.842920924169674,
7.59447542730139));
#10194=CARTESIAN_POINT('Ctrl Pts',(0.841321536411735,-0.406654290784301,
7.64086362524321));
#10195=CARTESIAN_POINT('Ctrl Pts',(0.909589372447933,0.206086771304483,
7.68719784696282));
#10196=CARTESIAN_POINT('Ctrl Pts',(0.618292515133597,0.668535774036831,
7.72832444946292));
#10197=CARTESIAN_POINT('Ctrl Pts',(0.200396624785897,0.868830700289083,
7.76426233212836));
#10198=CARTESIAN_POINT('Ctrl Pts',(-0.195890402329679,0.869105512774701,
7.79503036801838));
#10199=CARTESIAN_POINT('Ctrl Pts',(-0.552707853806054,0.697052799739259,
7.82575875672798));
#10200=CARTESIAN_POINT('Ctrl Pts',(-0.799378718992942,0.387911126397045,
7.85644623919681));
#10201=CARTESIAN_POINT('Ctrl Pts',(-0.886927475416378,0.00295721515884234,
7.88708853513497));
#10202=CARTESIAN_POINT('Ctrl Pts',(-0.785184349752334,-0.445993117087998,
7.92278375683408));
#10203=CARTESIAN_POINT('Ctrl Pts',(-0.402839530786299,-0.828885390140482,
7.96349431373723));
#10204=CARTESIAN_POINT('Ctrl Pts',(0.201302010936541,-0.896821923448385,
8.00917558757561));
#10205=CARTESIAN_POINT('Ctrl Pts',(0.713986287258037,-0.573914344502033,
8.05472562598296));
#10206=CARTESIAN_POINT('Ctrl Pts',(0.846713007247097,-0.194478858458525,
8.0850064631985));
#10207=CARTESIAN_POINT('Ctrl Pts',(0.846738971182356,-0.00398292970981142,
8.10012042772348));
#10208=CARTESIAN_POINT('Ctrl Pts',(0.817900488558397,0.00475133480574126,
6.79014507753449));
#10209=CARTESIAN_POINT('Ctrl Pts',(0.817875394277992,0.188866598068458,
6.80475279938448));
#10210=CARTESIAN_POINT('Ctrl Pts',(0.689784750139483,0.555422299671024,
6.8340140416451));
#10211=CARTESIAN_POINT('Ctrl Pts',(0.193435302274592,0.868118944792773,
6.87807729673241));
#10212=CARTESIAN_POINT('Ctrl Pts',(-0.293256146690176,0.812871758347855,
6.9149328617589));
#10213=CARTESIAN_POINT('Ctrl Pts',(-0.562009024419609,0.621358825924622,
6.94080240280578));
#10214=CARTESIAN_POINT('Ctrl Pts',(-0.682353384796979,0.478801116976173,
6.95560474741592));
#10215=CARTESIAN_POINT('Ctrl Pts',(-0.814675078268824,0.255341759501056,
6.97618178190882));
#10216=CARTESIAN_POINT('Ctrl Pts',(-0.860168272260483,-0.0497078330155523,
6.99968650056098));
#10217=CARTESIAN_POINT('Ctrl Pts',(-0.748436652472878,-0.411235760371946,
7.02944414274922));
#10218=CARTESIAN_POINT('Ctrl Pts',(-0.535961280579827,-0.678272766320467,
7.05594466708157));
#10219=CARTESIAN_POINT('Ctrl Pts',(-0.188978255123113,-0.845572124583574,
7.08582257562938));
#10220=CARTESIAN_POINT('Ctrl Pts',(0.13248022518062,-0.845505300794893,
7.11077362222657));
#10221=CARTESIAN_POINT('Ctrl Pts',(0.371055530451376,-0.761851985697717,
7.13076512684332));
#10222=CARTESIAN_POINT('Ctrl Pts',(0.585441233097604,-0.627371491436652,
7.15077683547094));
#10223=CARTESIAN_POINT('Ctrl Pts',(0.786808305815678,-0.375161061631681,
7.17582884965771));
#10224=CARTESIAN_POINT('Ctrl Pts',(0.87325510779514,0.00343457323490477,
7.20594902792096));
#10225=CARTESIAN_POINT('Ctrl Pts',(0.78686116127143,0.382313470509998,7.23612496849841));
#10226=CARTESIAN_POINT('Ctrl Pts',(0.517164760490624,0.721540784070928,
7.2697136876539));
#10227=CARTESIAN_POINT('Ctrl Pts',(0.147101057916398,0.86683917287086,7.30000372404372));
#10228=CARTESIAN_POINT('Ctrl Pts',(-0.237651739773033,0.837437753905466,
7.33034258187388));
#10229=CARTESIAN_POINT('Ctrl Pts',(-0.5512129818335,0.686952617632169,7.35734554941477));
#10230=CARTESIAN_POINT('Ctrl Pts',(-0.795631894615633,0.380338435114614,
7.38776877999359));
#10231=CARTESIAN_POINT('Ctrl Pts',(-0.898294846189099,-0.0662073699539118,
7.42331233504687));
#10232=CARTESIAN_POINT('Ctrl Pts',(-0.720507904090487,-0.577015468903857,
7.46400084949913));
#10233=CARTESIAN_POINT('Ctrl Pts',(-0.203663618176354,-0.901805888966958,
7.50985760554902));
#10234=CARTESIAN_POINT('Ctrl Pts',(0.403204771572536,-0.833486961268272,
7.55578804854158));
#10235=CARTESIAN_POINT('Ctrl Pts',(0.836365154142795,-0.401111707981145,
7.60178359598158));
#10236=CARTESIAN_POINT('Ctrl Pts',(0.904471271556475,0.207858603382153,
7.6478348461097));
#10237=CARTESIAN_POINT('Ctrl Pts',(0.614428615698172,0.668722267241424,
7.68881129227799));
#10238=CARTESIAN_POINT('Ctrl Pts',(0.197261178437678,0.868767690888966,
7.7246899075929));
#10239=CARTESIAN_POINT('Ctrl Pts',(-0.199005609016601,0.869111738380501,
7.7554569214687));
#10240=CARTESIAN_POINT('Ctrl Pts',(-0.556427435495044,0.696852222393774,
7.78623527481754));
#10241=CARTESIAN_POINT('Ctrl Pts',(-0.803949133824011,0.38676076397028,
7.81702187878289));
#10242=CARTESIAN_POINT('Ctrl Pts',(-0.891995003933998,-5.28792355482503E-5,
7.84781415673619));
#10243=CARTESIAN_POINT('Ctrl Pts',(-0.789679403174556,-0.4519291484846,
7.88374203453794));
#10244=CARTESIAN_POINT('Ctrl Pts',(-0.404226672020434,-0.838247889347281,
7.9248014076827));
#10245=CARTESIAN_POINT('Ctrl Pts',(0.206521632311494,-0.907164419165389,
7.97098703818337));
#10246=CARTESIAN_POINT('Ctrl Pts',(0.726215048173051,-0.580160328067018,
8.01714652643371));
#10247=CARTESIAN_POINT('Ctrl Pts',(0.86119627917958,-0.194707506801938,
8.04791285500075));
#10248=CARTESIAN_POINT('Ctrl Pts',(0.861222672429394,-0.00106172137465173,
8.0632767294446));
#10249=CARTESIAN_POINT('Ctrl Pts',(0.799992192036797,0.00474896193479852,
6.79014422086044));
#10250=CARTESIAN_POINT('Ctrl Pts',(0.799967638550529,0.184896450338747,
6.80443713908974));
#10251=CARTESIAN_POINT('Ctrl Pts',(0.674670361705441,0.543455008309391,
6.8330594352144));
#10252=CARTESIAN_POINT('Ctrl Pts',(0.189034209544693,0.849439608053688,
6.87617354971506));
#10253=CARTESIAN_POINT('Ctrl Pts',(-0.287258299249701,0.795379885058583,
6.91224027998794));
#10254=CARTESIAN_POINT('Ctrl Pts',(-0.550325497980241,0.607926215999118,
6.93756224237155));
#10255=CARTESIAN_POINT('Ctrl Pts',(-0.668135787638992,0.468370262290034,
6.95205278987894));
#10256=CARTESIAN_POINT('Ctrl Pts',(-0.797681515793003,0.249601245171223,
6.97219797725517));
#10257=CARTESIAN_POINT('Ctrl Pts',(-0.842241289744138,-0.0491002547813337,
6.99521334099182));
#10258=CARTESIAN_POINT('Ctrl Pts',(-0.732812122296168,-0.403197173369283,
7.02435916833342));
#10259=CARTESIAN_POINT('Ctrl Pts',(-0.524668382980495,-0.664806008100517,
7.0503201318013));
#10260=CARTESIAN_POINT('Ctrl Pts',(-0.184652568425117,-0.828760962866216,
7.07959861118036));
#10261=CARTESIAN_POINT('Ctrl Pts',(0.130453782933179,-0.82870656943649,
7.10405631433573));
#10262=CARTESIAN_POINT('Ctrl Pts',(0.364375751582702,-0.746687575144636,
7.12365775087804));
#10263=CARTESIAN_POINT('Ctrl Pts',(0.574616121324387,-0.614810215974657,
7.14328235821488));
#10264=CARTESIAN_POINT('Ctrl Pts',(0.772150732123964,-0.367420603086453,
7.16785616546509));
#10265=CARTESIAN_POINT('Ctrl Pts',(0.856997117769862,0.00408861547259015,
7.19741267271575));
#10266=CARTESIAN_POINT('Ctrl Pts',(0.772201652552023,0.376032772307348,
7.22703591400899));
#10267=CARTESIAN_POINT('Ctrl Pts',(0.507351873091063,0.709199534687239,
7.26002305113266));
#10268=CARTESIAN_POINT('Ctrl Pts',(0.143736848284574,0.852002078379093,
7.28978615651597));
#10269=CARTESIAN_POINT('Ctrl Pts',(-0.234502546384647,0.823108658745492,
7.31961111148852));
#10270=CARTESIAN_POINT('Ctrl Pts',(-0.542883282495364,0.675129422402413,
7.34616719094667));
#10271=CARTESIAN_POINT('Ctrl Pts',(-0.783396359273759,0.37345029211527,
7.3761020331664));
#10272=CARTESIAN_POINT('Ctrl Pts',(-0.884489493081995,-0.0661466723839558,
7.41109301032321));
#10273=CARTESIAN_POINT('Ctrl Pts',(-0.709418296017906,-0.569369739308696,
7.45117535759087));
#10274=CARTESIAN_POINT('Ctrl Pts',(-0.19989068769657,-0.889667511851702,
7.49638689971083));
#10275=CARTESIAN_POINT('Ctrl Pts',(0.398973895326053,-0.822339305277361,
7.54171055210185));
#10276=CARTESIAN_POINT('Ctrl Pts',(0.826865587387622,-0.395358142551438,
7.58713932258037));
#10277=CARTESIAN_POINT('Ctrl Pts',(0.894293657405342,0.206666783144423,
7.6326658525427));
#10278=CARTESIAN_POINT('Ctrl Pts',(0.607352590357856,0.662764035303079,
7.67321405418637));
#10279=CARTESIAN_POINT('Ctrl Pts',(0.194215191945802,0.860916697467946,
7.70874703376387));
#10280=CARTESIAN_POINT('Ctrl Pts',(-0.198496552114366,0.86128604965953,
7.7392380606388));
#10281=CARTESIAN_POINT('Ctrl Pts',(-0.552965374281963,0.690483866395827,
7.76976084505319));
#10282=CARTESIAN_POINT('Ctrl Pts',(-0.798625493103115,0.382774108679761,
7.80031292414605));
#10283=CARTESIAN_POINT('Ctrl Pts',(-0.886090514398701,-0.00135276288038935,
7.83089169974969));
#10284=CARTESIAN_POINT('Ctrl Pts',(-0.784450923473031,-0.450417071001065,
7.86659566812776));
#10285=CARTESIAN_POINT('Ctrl Pts',(-0.401130832210515,-0.834733160113732,
7.90743505712395));
#10286=CARTESIAN_POINT('Ctrl Pts',(0.206987829997999,-0.903462960885791,
7.95342319362056));
#10287=CARTESIAN_POINT('Ctrl Pts',(0.725081242328631,-0.57760276120548,
7.99943459556092));
#10288=CARTESIAN_POINT('Ctrl Pts',(0.859845779758374,-0.192969267412252,
8.03013735189051));
#10289=CARTESIAN_POINT('Ctrl Pts',(0.85987212861708,0.000350822954683268,
8.04547538565828));
#10290=CARTESIAN_POINT('',(0.740013321878819,-3.30221092258282E-6,6.84996753665487));
#10291=CARTESIAN_POINT('',(0.86002906121511,-2.8436073730086E-6,6.85013896332608));
#10292=CARTESIAN_POINT('Ctrl Pts',(0.740023219291072,-5.77198260618599E-6,
6.85002034628079));
#10293=CARTESIAN_POINT('Ctrl Pts',(0.740021358405138,-2.10300419701926E-5,
6.85039822499709));
#10294=CARTESIAN_POINT('Ctrl Pts',(0.740023024222631,-3.62850179820163E-5,
6.85077606240544));
#10295=CARTESIAN_POINT('Ctrl Pts',(0.740028231502145,-5.1534688844035E-5,
6.85115380766388));
#10296=CARTESIAN_POINT('Ctrl Pts',(0.740085053936413,-0.00021794085503002,
6.85527580746438));
#10297=CARTESIAN_POINT('Ctrl Pts',(0.740561847799387,-0.00038290723370555,
6.85936598291913));
#10298=CARTESIAN_POINT('Ctrl Pts',(0.741474476273296,-0.00054348152203615,
6.86335924813516));
#10299=CARTESIAN_POINT('Ctrl Pts',(0.742233180141228,-0.000676973229921408,
6.86667900623136));
#10300=CARTESIAN_POINT('Ctrl Pts',(0.743293477943993,-0.000807438902367973,
6.86993201105744));
#10301=CARTESIAN_POINT('Ctrl Pts',(0.744631277735025,-0.000933850565882489,
6.87308796691842));
#10302=CARTESIAN_POINT('Ctrl Pts',(0.746754426168902,-0.00113447156105222,
6.8780966108041));
#10303=CARTESIAN_POINT('Ctrl Pts',(0.749546546792157,-0.00132241308026135,
6.88279723847818));
#10304=CARTESIAN_POINT('Ctrl Pts',(0.752899116929639,-0.00149305386639579,
6.88707335410488));
#10305=CARTESIAN_POINT('Ctrl Pts',(0.754360743054021,-0.00156744844150423,
6.88893762004252));
#10306=CARTESIAN_POINT('Ctrl Pts',(0.755929524328344,-0.00163854499625076,
6.89072092401184));
#10307=CARTESIAN_POINT('Ctrl Pts',(0.757598887046534,-0.00170586425030808,
6.89241168757878));
#10308=CARTESIAN_POINT('Ctrl Pts',(0.761394051663765,-0.001858909270586,
6.89625550533956));
#10309=CARTESIAN_POINT('Ctrl Pts',(0.765657159823746,-0.00199058430570913,
6.89957326466661));
#10310=CARTESIAN_POINT('Ctrl Pts',(0.770297905279784,-0.00209437976410097,
6.90224220648893));
#10311=CARTESIAN_POINT('Ctrl Pts',(0.771480718348967,-0.00212083470024662,
6.9029224548021));
#10312=CARTESIAN_POINT('Ctrl Pts',(0.772688227465772,-0.00214546614515498,
6.90356035260593));
#10313=CARTESIAN_POINT('Ctrl Pts',(0.773919225517153,-0.00216813570411822,
6.90415338933386));
#10314=CARTESIAN_POINT('Ctrl Pts',(0.774849981021487,-0.00218527611856664,
6.90460178338141));
#10315=CARTESIAN_POINT('Ctrl Pts',(0.77579416755915,-0.00220129455406626,
6.90502452541544));
#10316=CARTESIAN_POINT('Ctrl Pts',(0.77675073101501,-0.0022162186817045,
6.90542159869653));
#10317=CARTESIAN_POINT('Ctrl Pts',(0.781727100262787,-0.0022938590822172,
6.90748730929108));
#10318=CARTESIAN_POINT('Ctrl Pts',(0.786971413210206,-0.00234111121487575,
6.90883536506399));
#10319=CARTESIAN_POINT('Ctrl Pts',(0.792325599468412,-0.00236147596166846,
6.90948862972605));
#10320=CARTESIAN_POINT('Ctrl Pts',(0.794699452788802,-0.00237050495682504,
6.90977826374556));
#10321=CARTESIAN_POINT('Ctrl Pts',(0.797095176688634,-0.00237419920632471,
6.90993065281261));
#10322=CARTESIAN_POINT('Ctrl Pts',(0.799499433912905,-0.00237262251695804,
6.90994459926205));
#10323=CARTESIAN_POINT('Ctrl Pts',(0.804934689322609,-0.00236905812737313,
6.90997612771666));
#10324=CARTESIAN_POINT('Ctrl Pts',(0.810341856817132,-0.00233882740457025,
6.909303140357));
#10325=CARTESIAN_POINT('Ctrl Pts',(0.815566649891691,-0.00228184659800146,
6.90793064851273));
#10326=CARTESIAN_POINT('Ctrl Pts',(0.817867829031793,-0.00225675028479036,
6.90732615574968));
#10327=CARTESIAN_POINT('Ctrl Pts',(0.820133625359067,-0.00222640701590779,
6.90658530716917));
#10328=CARTESIAN_POINT('Ctrl Pts',(0.822349983198305,-0.00219053233431339,
6.90570540025299));
#10329=CARTESIAN_POINT('Ctrl Pts',(0.823602413960143,-0.00217026008675276,
6.90520817797694));
#10330=CARTESIAN_POINT('Ctrl Pts',(0.82483494206673,-0.00214828094937227,
6.90466814014931));
#10331=CARTESIAN_POINT('Ctrl Pts',(0.826045257442232,-0.00212456411533838,
6.90408538174413));
#10332=CARTESIAN_POINT('Ctrl Pts',(0.830894037694746,-0.0020295494449117,
6.90175072789755));
#10333=CARTESIAN_POINT('Ctrl Pts',(0.835388487964696,-0.00190698894305515,
6.89873407321304));
#10334=CARTESIAN_POINT('Ctrl Pts',(0.839441071831611,-0.00176396566847474,
6.89516397873058));
#10335=CARTESIAN_POINT('Ctrl Pts',(0.840235771719969,-0.001735919221054,
6.89446389360469));
#10336=CARTESIAN_POINT('Ctrl Pts',(0.841013384724027,-0.00170707348974732,
6.89374239738474));
#10337=CARTESIAN_POINT('Ctrl Pts',(0.841773092391,-0.00167746545197683,
6.89300029288931));
#10338=CARTESIAN_POINT('Ctrl Pts',(0.845672921400161,-0.00152547766822612,
6.88919082674212));
#10339=CARTESIAN_POINT('Ctrl Pts',(0.84905256830136,-0.00135568308239744,
6.88489142900407));
#10340=CARTESIAN_POINT('Ctrl Pts',(0.851819498119605,-0.00117319323714043,
6.88022796254556));
#10341=CARTESIAN_POINT('Ctrl Pts',(0.853029466194191,-0.00109339110943874,
6.87818864608206));
#10342=CARTESIAN_POINT('Ctrl Pts',(0.854121791492832,-0.0010111142513845,
6.8760792357492));
#10343=CARTESIAN_POINT('Ctrl Pts',(0.855085995445545,-0.0009266211082642,
6.87390868773667));
#10344=CARTESIAN_POINT('Ctrl Pts',(0.85659857140088,-0.000794074154567515,
6.87050368330332));
#10345=CARTESIAN_POINT('Ctrl Pts',(0.85778271855372,-0.000657301396693565,
6.86697912957925));
#10346=CARTESIAN_POINT('Ctrl Pts',(0.858606344933536,-0.000517333545493498,
6.86337295784898));
#10347=CARTESIAN_POINT('Ctrl Pts',(0.859509064743485,-0.000363924481468129,
6.8594204828691));
#10348=CARTESIAN_POINT('Ctrl Pts',(0.859979039725546,-0.000206633239390191,
6.85536955609449));
#10349=CARTESIAN_POINT('Ctrl Pts',(0.860033114959129,-4.77911640563713E-5,
6.85128419258908));
#10350=CARTESIAN_POINT('Ctrl Pts',(0.860038121181873,-3.30857479617889E-5,
6.85090597434861));
#10351=CARTESIAN_POINT('Ctrl Pts',(0.860039548467556,-1.83741767728084E-5,
6.85052764184536));
#10352=CARTESIAN_POINT('Ctrl Pts',(0.860037413159089,-3.65835365705083E-6,
6.85014924671004));
#10353=CARTESIAN_POINT('',(0.799999353205575,0.00474549275567414,6.79018795858619));
#10354=CARTESIAN_POINT('Origin',(0.8,3.02639196116122E-20,6.85));
#10355=CARTESIAN_POINT('',(0.859872007312157,8.03685277434799E-7,8.04544761499495));
#10356=CARTESIAN_POINT('Ctrl Pts',(0.799992192036797,0.00474896193479852,
6.79014422086044));
#10357=CARTESIAN_POINT('Ctrl Pts',(0.799967638550529,0.184896450338747,
6.80443713908974));
#10358=CARTESIAN_POINT('Ctrl Pts',(0.674670361705441,0.543455008309391,
6.8330594352144));
#10359=CARTESIAN_POINT('Ctrl Pts',(0.189034209544693,0.849439608053688,
6.87617354971506));
#10360=CARTESIAN_POINT('Ctrl Pts',(-0.287258299249701,0.795379885058583,
6.91224027998794));
#10361=CARTESIAN_POINT('Ctrl Pts',(-0.550325497980241,0.607926215999118,
6.93756224237155));
#10362=CARTESIAN_POINT('Ctrl Pts',(-0.668135787638992,0.468370262290034,
6.95205278987894));
#10363=CARTESIAN_POINT('Ctrl Pts',(-0.797681515793003,0.249601245171223,
6.97219797725517));
#10364=CARTESIAN_POINT('Ctrl Pts',(-0.842241289744138,-0.0491002547813337,
6.99521334099182));
#10365=CARTESIAN_POINT('Ctrl Pts',(-0.732812122296168,-0.403197173369283,
7.02435916833342));
#10366=CARTESIAN_POINT('Ctrl Pts',(-0.524668382980495,-0.664806008100517,
7.0503201318013));
#10367=CARTESIAN_POINT('Ctrl Pts',(-0.184652568425117,-0.828760962866216,
7.07959861118036));
#10368=CARTESIAN_POINT('Ctrl Pts',(0.130453782933179,-0.82870656943649,
7.10405631433573));
#10369=CARTESIAN_POINT('Ctrl Pts',(0.364375751582702,-0.746687575144636,
7.12365775087804));
#10370=CARTESIAN_POINT('Ctrl Pts',(0.574616121324387,-0.614810215974657,
7.14328235821488));
#10371=CARTESIAN_POINT('Ctrl Pts',(0.772150732123964,-0.367420603086453,
7.16785616546509));
#10372=CARTESIAN_POINT('Ctrl Pts',(0.856997117769862,0.00408861547259015,
7.19741267271575));
#10373=CARTESIAN_POINT('Ctrl Pts',(0.772201652552023,0.376032772307348,
7.22703591400899));
#10374=CARTESIAN_POINT('Ctrl Pts',(0.507351873091063,0.709199534687239,
7.26002305113266));
#10375=CARTESIAN_POINT('Ctrl Pts',(0.143736848284574,0.852002078379093,
7.28978615651597));
#10376=CARTESIAN_POINT('Ctrl Pts',(-0.234502546384647,0.823108658745492,
7.31961111148852));
#10377=CARTESIAN_POINT('Ctrl Pts',(-0.542883282495364,0.675129422402413,
7.34616719094667));
#10378=CARTESIAN_POINT('Ctrl Pts',(-0.783396359273759,0.37345029211527,
7.3761020331664));
#10379=CARTESIAN_POINT('Ctrl Pts',(-0.884489493081995,-0.0661466723839558,
7.41109301032321));
#10380=CARTESIAN_POINT('Ctrl Pts',(-0.709418296017906,-0.569369739308696,
7.45117535759087));
#10381=CARTESIAN_POINT('Ctrl Pts',(-0.19989068769657,-0.889667511851702,
7.49638689971083));
#10382=CARTESIAN_POINT('Ctrl Pts',(0.398973895326053,-0.822339305277361,
7.54171055210185));
#10383=CARTESIAN_POINT('Ctrl Pts',(0.826865587387622,-0.395358142551438,
7.58713932258037));
#10384=CARTESIAN_POINT('Ctrl Pts',(0.894293657405342,0.206666783144423,
7.6326658525427));
#10385=CARTESIAN_POINT('Ctrl Pts',(0.607352590357856,0.662764035303079,
7.67321405418637));
#10386=CARTESIAN_POINT('Ctrl Pts',(0.194215191945802,0.860916697467946,
7.70874703376387));
#10387=CARTESIAN_POINT('Ctrl Pts',(-0.198496552114366,0.86128604965953,
7.7392380606388));
#10388=CARTESIAN_POINT('Ctrl Pts',(-0.552965374281963,0.690483866395827,
7.76976084505319));
#10389=CARTESIAN_POINT('Ctrl Pts',(-0.798625493103115,0.382774108679761,
7.80031292414605));
#10390=CARTESIAN_POINT('Ctrl Pts',(-0.886090514398701,-0.00135276288038935,
7.83089169974969));
#10391=CARTESIAN_POINT('Ctrl Pts',(-0.784450923473031,-0.450417071001065,
7.86659566812776));
#10392=CARTESIAN_POINT('Ctrl Pts',(-0.401130832210515,-0.834733160113732,
7.90743505712395));
#10393=CARTESIAN_POINT('Ctrl Pts',(0.206987829997999,-0.903462960885791,
7.95342319362056));
#10394=CARTESIAN_POINT('Ctrl Pts',(0.724977015357669,-0.577668315834745,
7.99942533925898));
#10395=CARTESIAN_POINT('Ctrl Pts',(0.859764427178652,-0.19320138704919,
8.03011882209587));
#10396=CARTESIAN_POINT('Ctrl Pts',(0.859872007312956,8.05120031746468E-7,
8.04544761510878));
#10397=CARTESIAN_POINT('Ctrl Pts',(0.859872007312157,8.03685277532201E-7,
8.04544761499494));
#10398=CARTESIAN_POINT('Ctrl Pts',(0.859872039269663,5.81957034837644E-5,
8.04545216851661));
#10399=CARTESIAN_POINT('Ctrl Pts',(0.859872065291453,0.000115587812293562,
8.0454567220371));
#10400=CARTESIAN_POINT('Ctrl Pts',(0.859872085377142,0.000172980010638188,
8.04546127555641));
#10401=CARTESIAN_POINT('Origin',(0.8,3.02639196116122E-20,6.85));
#10402=CARTESIAN_POINT('Origin',(0.8,-3.5,6.85));
#10403=CARTESIAN_POINT('Origin',(0.8,0.,6.85));
#10404=CARTESIAN_POINT('',(0.74,-3.5,6.85));
#10405=CARTESIAN_POINT('',(0.74,-3.5,6.85));
#10406=CARTESIAN_POINT('Origin',(0.8,-3.5,6.85));
#10407=CARTESIAN_POINT('Origin',(0.8,0.,6.85));
#10408=CARTESIAN_POINT('',(0.8,0.,6.85));
#10409=CARTESIAN_POINT('Origin',(0.8,-3.5,6.85));
#10410=CARTESIAN_POINT('Origin',(0.8,3.02639196116122E-20,6.85));
#10411=CARTESIAN_POINT('',(0.,0.,0.));
#10412=CARTESIAN_POINT('Origin',(6.,1.9,-0.1));
#10413=CARTESIAN_POINT('',(5.835,1.9,0.));
#10414=CARTESIAN_POINT('Origin',(6.,1.9,0.));
#10415=CARTESIAN_POINT('',(5.835,1.9,1.1));
#10416=CARTESIAN_POINT('',(5.835,1.9,-0.1));
#10417=CARTESIAN_POINT('Origin',(6.,1.9,1.1));
#10418=CARTESIAN_POINT('Origin',(6.,1.9,1.1));
#10419=CARTESIAN_POINT('Origin',(6.,1.4,5.5));
#10420=CARTESIAN_POINT('',(5.79,1.5,5.5));
#10421=CARTESIAN_POINT('Origin',(6.,1.5,5.5));
#10422=CARTESIAN_POINT('',(5.79,2.3,5.5));
#10423=CARTESIAN_POINT('',(5.79,1.4,5.5));
#10424=CARTESIAN_POINT('Origin',(6.,2.3,5.5));
#10425=CARTESIAN_POINT('Origin',(7.,2.3,0.));
#10426=CARTESIAN_POINT('',(7.,2.3,0.));
#10427=CARTESIAN_POINT('',(5.,2.3,0.));
#10428=CARTESIAN_POINT('',(7.,2.3,0.));
#10429=CARTESIAN_POINT('',(5.,2.3,6.5));
#10430=CARTESIAN_POINT('',(5.,2.3,0.));
#10431=CARTESIAN_POINT('',(7.,2.3,6.5));
#10432=CARTESIAN_POINT('',(7.,2.3,6.5));
#10433=CARTESIAN_POINT('',(7.,2.3,0.));
#10434=CARTESIAN_POINT('Origin',(7.,1.5,0.));
#10435=CARTESIAN_POINT('',(7.,1.5,0.));
#10436=CARTESIAN_POINT('',(7.,1.5,0.));
#10437=CARTESIAN_POINT('',(7.,1.5,6.5));
#10438=CARTESIAN_POINT('',(7.,1.5,6.5));
#10439=CARTESIAN_POINT('',(7.,1.5,0.));
#10440=CARTESIAN_POINT('Origin',(5.,1.5,0.));
#10441=CARTESIAN_POINT('',(5.,1.5,0.));
#10442=CARTESIAN_POINT('',(5.,1.5,0.));
#10443=CARTESIAN_POINT('',(5.,1.5,6.5));
#10444=CARTESIAN_POINT('',(5.,1.5,6.5));
#10445=CARTESIAN_POINT('',(5.,1.5,0.));
#10446=CARTESIAN_POINT('Origin',(5.,2.3,0.));
#10447=CARTESIAN_POINT('',(5.,2.3,0.));
#10448=CARTESIAN_POINT('',(5.,2.3,6.5));
#10449=CARTESIAN_POINT('Origin',(6.,1.9,6.5));
#10450=CARTESIAN_POINT('Origin',(6.,1.9,0.));
#10451=CARTESIAN_POINT('',(0.,0.,0.));
#10452=CARTESIAN_POINT('Origin',(0.,0.09,0.));
#10453=CARTESIAN_POINT('',(-0.285,0.1,3.49024337756996E-17));
#10454=CARTESIAN_POINT('Origin',(0.,0.1,0.));
#10455=CARTESIAN_POINT('',(-0.265,0.08,-3.24531401774049E-17));
#10456=CARTESIAN_POINT('',(-0.275,0.09,3.36777869765522E-17));
#10457=CARTESIAN_POINT('Origin',(0.,0.08,0.));
#10458=CARTESIAN_POINT('Origin',(0.,0.,0.));
#10459=CARTESIAN_POINT('',(-0.265,0.,3.24531401774049E-17));
#10460=CARTESIAN_POINT('',(-0.265,0.,3.24531401774049E-17));
#10461=CARTESIAN_POINT('Origin',(0.,0.,0.));
#10462=CARTESIAN_POINT('Origin',(0.,0.1,0.));
#10463=CARTESIAN_POINT('',(-0.5,0.1,6.12323399573677E-17));
#10464=CARTESIAN_POINT('Origin',(0.,0.1,0.));
#10465=CARTESIAN_POINT('Origin',(0.,0.,0.));
#10466=CARTESIAN_POINT('',(-0.5,0.,6.12323399573677E-17));
#10467=CARTESIAN_POINT('',(-0.5,0.,6.12323399573677E-17));
#10468=CARTESIAN_POINT('Origin',(0.,0.,0.));
#10469=CARTESIAN_POINT('Origin',(0.,0.,0.));
#10470=CARTESIAN_POINT('',(0.,0.,0.));
#10471=CARTESIAN_POINT('Origin',(0.375,0.5,0.));
#10472=CARTESIAN_POINT('',(-0.375,0.5,-4.59242549680257E-17));
#10473=CARTESIAN_POINT('Origin',(0.,0.5,0.));
#10474=CARTESIAN_POINT('Origin',(0.,0.475,0.));
#10475=CARTESIAN_POINT('',(-0.425,0.45,-5.20474889637625E-17));
#10476=CARTESIAN_POINT('Origin',(0.,0.45,0.));
#10477=CARTESIAN_POINT('',(-0.4,0.475,-4.89858719658941E-17));
#10478=CARTESIAN_POINT('Origin',(0.,0.24,0.));
#10479=CARTESIAN_POINT('',(-0.425,0.0299999999999998,-5.20474889637625E-17));
#10480=CARTESIAN_POINT('Origin',(0.,0.0299999999999998,0.));
#10481=CARTESIAN_POINT('',(-0.425,0.24,-5.20474889637625E-17));
#10482=CARTESIAN_POINT('Origin',(0.,0.0150000000000001,0.));
#10483=CARTESIAN_POINT('',(-0.395,4.85722573273506E-17,-4.83735485663204E-17));
#10484=CARTESIAN_POINT('Origin',(0.,0.,0.));
#10485=CARTESIAN_POINT('',(-0.41,0.0150000000000001,-5.02105187650415E-17));
#10486=CARTESIAN_POINT('Origin',(0.27,0.,0.));
#10487=CARTESIAN_POINT('',(-0.27,0.,-3.30654635769785E-17));
#10488=CARTESIAN_POINT('Origin',(0.,0.,0.));
#10489=CARTESIAN_POINT('Origin',(0.,-0.02,0.));
#10490=CARTESIAN_POINT('',(-0.24505,-0.0498999999999999,3.00099698131059E-17));
#10491=CARTESIAN_POINT('Origin',(0.,-0.0498999999999999,0.));
#10492=CARTESIAN_POINT('',(-0.26,-0.02,-3.18408167778312E-17));
#10493=CARTESIAN_POINT('Origin',(0.,-0.995,0.));
#10494=CARTESIAN_POINT('',(-0.24505,-1.95495,3.00099698131059E-17));
#10495=CARTESIAN_POINT('Origin',(0.,-1.95495,0.));
#10496=CARTESIAN_POINT('',(-0.24505,-0.995,-3.00099698131059E-17));
#10497=CARTESIAN_POINT('Origin',(0.,-1.975,0.));
#10498=CARTESIAN_POINT('',(-0.2,-2.,-2.44929359829471E-17));
#10499=CARTESIAN_POINT('Origin',(0.,-2.,0.));
#10500=CARTESIAN_POINT('',(-0.225,-1.975,-2.75545529808154E-17));
#10501=CARTESIAN_POINT('Origin',(0.,-2.,0.));
#10502=CARTESIAN_POINT('Origin',(0.115470053837925,-0.5,-0.2));
#10503=CARTESIAN_POINT('',(0.23094010767585,-0.5,0.));
#10504=CARTESIAN_POINT('',(0.115470053837925,-0.5,-0.2));
#10505=CARTESIAN_POINT('',(0.23094010767585,-0.5,0.));
#10506=CARTESIAN_POINT('',(0.115470053837925,-0.8,-0.2));
#10507=CARTESIAN_POINT('',(0.115470053837925,-0.5,-0.2));
#10508=CARTESIAN_POINT('',(0.23094010767585,-0.8,0.));
#10509=CARTESIAN_POINT('',(0.23094010767585,-0.8,0.));
#10510=CARTESIAN_POINT('',(0.23094010767585,-0.5,0.));
#10511=CARTESIAN_POINT('Origin',(-0.115470053837925,-0.5,-0.2));
#10512=CARTESIAN_POINT('',(-0.115470053837925,-0.5,-0.2));
#10513=CARTESIAN_POINT('',(0.115470053837925,-0.5,-0.2));
#10514=CARTESIAN_POINT('',(-0.115470053837925,-0.8,-0.2));
#10515=CARTESIAN_POINT('',(-0.115470053837925,-0.5,-0.2));
#10516=CARTESIAN_POINT('',(0.115470053837925,-0.8,-0.2));
#10517=CARTESIAN_POINT('Origin',(-0.23094010767585,-0.5,-2.77555756156289E-17));
#10518=CARTESIAN_POINT('',(-0.23094010767585,-0.5,-2.82820063659975E-17));
#10519=CARTESIAN_POINT('',(-0.115470053837925,-0.5,-0.2));
#10520=CARTESIAN_POINT('',(-0.23094010767585,-0.8,-2.77555756156289E-17));
#10521=CARTESIAN_POINT('',(-0.23094010767585,-0.5,-2.82820063659975E-17));
#10522=CARTESIAN_POINT('',(-0.115470053837925,-0.8,-0.2));
#10523=CARTESIAN_POINT('Origin',(-0.115470053837925,-0.5,0.2));
#10524=CARTESIAN_POINT('',(-0.115470053837925,-0.5,0.2));
#10525=CARTESIAN_POINT('',(-0.23094010767585,-0.5,-2.82820063659975E-17));
#10526=CARTESIAN_POINT('',(-0.115470053837925,-0.8,0.2));
#10527=CARTESIAN_POINT('',(-0.115470053837925,-0.5,0.2));
#10528=CARTESIAN_POINT('',(-0.23094010767585,-0.8,-2.82820063659975E-17));
#10529=CARTESIAN_POINT('Origin',(0.115470053837925,-0.5,0.2));
#10530=CARTESIAN_POINT('',(0.115470053837925,-0.5,0.2));
#10531=CARTESIAN_POINT('',(-0.115470053837925,-0.5,0.2));
#10532=CARTESIAN_POINT('',(0.115470053837925,-0.8,0.2));
#10533=CARTESIAN_POINT('',(0.115470053837925,-0.5,0.2));
#10534=CARTESIAN_POINT('',(-0.115470053837925,-0.8,0.2));
#10535=CARTESIAN_POINT('Origin',(0.23094010767585,-0.5,0.));
#10536=CARTESIAN_POINT('',(0.115470053837925,-0.5,0.2));
#10537=CARTESIAN_POINT('',(0.115470053837925,-0.8,0.2));
#10538=CARTESIAN_POINT('Origin',(0.,-0.5,0.));
#10539=CARTESIAN_POINT('Origin',(0.,-0.8,0.));
#10540=CARTESIAN_POINT('',(0.,0.,0.));
#10541=CARTESIAN_POINT('Origin',(0.,0.0525042956467857,0.));
#10542=CARTESIAN_POINT('',(-0.230940107675851,0.0472735643746089,0.4));
#10543=CARTESIAN_POINT('',(0.23094010767585,0.0472735643746089,0.4));
#10544=CARTESIAN_POINT('Ctrl Pts',(-0.230940107675851,0.0472735643746089,
0.4));
#10545=CARTESIAN_POINT('Ctrl Pts',(1.11022302462516E-16,-0.0193931022920578,
0.4));
#10546=CARTESIAN_POINT('Ctrl Pts',(0.23094010767585,0.0472735643746089,
0.4));
#10547=CARTESIAN_POINT('',(-0.461880215351701,0.0472735643746089,-5.6564012731995E-17));
#10548=CARTESIAN_POINT('Ctrl Pts',(-0.461880215351701,0.0472735643746089,
-5.6564012731995E-17));
#10549=CARTESIAN_POINT('Ctrl Pts',(-0.346410161513776,-0.0193931022920579,
0.2));
#10550=CARTESIAN_POINT('Ctrl Pts',(-0.230940107675851,0.0472735643746089,
0.4));
#10551=CARTESIAN_POINT('',(-0.38,-2.08166817117217E-17,-4.65365783675994E-17));
#10552=CARTESIAN_POINT('',(-0.47094010767585,0.0525042956467857,-5.7673529545534E-17));
#10553=CARTESIAN_POINT('Origin',(0.,0.,0.));
#10554=CARTESIAN_POINT('',(-0.23094010767585,0.0472735643746089,-0.4));
#10555=CARTESIAN_POINT('Ctrl Pts',(-0.23094010767585,0.0472735643746089,
-0.4));
#10556=CARTESIAN_POINT('Ctrl Pts',(-0.346410161513775,-0.0193931022920578,
-0.2));
#10557=CARTESIAN_POINT('Ctrl Pts',(-0.461880215351701,0.0472735643746089,
-5.6564012731995E-17));
#10558=CARTESIAN_POINT('',(0.23094010767585,0.0472735643746089,-0.4));
#10559=CARTESIAN_POINT('Ctrl Pts',(0.23094010767585,0.0472735643746089,
-0.4));
#10560=CARTESIAN_POINT('Ctrl Pts',(0.,-0.0193931022920578,-0.4));
#10561=CARTESIAN_POINT('Ctrl Pts',(-0.23094010767585,0.0472735643746089,
-0.4));
#10562=CARTESIAN_POINT('',(0.461880215351701,0.0472735643746089,0.));
#10563=CARTESIAN_POINT('Ctrl Pts',(0.461880215351701,0.0472735643746089,
0.));
#10564=CARTESIAN_POINT('Ctrl Pts',(0.346410161513776,-0.019393102292058,
-0.2));
#10565=CARTESIAN_POINT('Ctrl Pts',(0.23094010767585,0.0472735643746089,
-0.4));
#10566=CARTESIAN_POINT('Ctrl Pts',(0.23094010767585,0.0472735643746089,
0.4));
#10567=CARTESIAN_POINT('Ctrl Pts',(0.346410161513776,-0.0193931022920577,
0.2));
#10568=CARTESIAN_POINT('Ctrl Pts',(0.461880215351701,0.0472735643746089,
0.));
#10569=CARTESIAN_POINT('Origin',(0.,0.417495704353214,0.));
#10570=CARTESIAN_POINT('',(-0.38,0.47,-4.65365783675994E-17));
#10571=CARTESIAN_POINT('Origin',(0.,0.47,0.));
#10572=CARTESIAN_POINT('',(-0.461880215351701,0.422726435625391,-5.6564012731995E-17));
#10573=CARTESIAN_POINT('',(-0.47094010767585,0.417495704353214,-5.7673529545534E-17));
#10574=CARTESIAN_POINT('',(-0.230940107675851,0.422726435625391,0.4));
#10575=CARTESIAN_POINT('Ctrl Pts',(-0.230940107675851,0.422726435625391,
0.4));
#10576=CARTESIAN_POINT('Ctrl Pts',(-0.346410161513776,0.489393102292058,
0.2));
#10577=CARTESIAN_POINT('Ctrl Pts',(-0.461880215351701,0.422726435625391,
-5.6564012731995E-17));
#10578=CARTESIAN_POINT('',(0.23094010767585,0.422726435625391,0.4));
#10579=CARTESIAN_POINT('Ctrl Pts',(0.23094010767585,0.422726435625391,0.4));
#10580=CARTESIAN_POINT('Ctrl Pts',(8.32667268468867E-17,0.489393102292058,
0.4));
#10581=CARTESIAN_POINT('Ctrl Pts',(-0.230940107675851,0.422726435625391,
0.4));
#10582=CARTESIAN_POINT('',(0.461880215351701,0.422726435625391,0.));
#10583=CARTESIAN_POINT('Ctrl Pts',(0.461880215351701,0.422726435625391,
0.));
#10584=CARTESIAN_POINT('Ctrl Pts',(0.346410161513776,0.489393102292058,
0.2));
#10585=CARTESIAN_POINT('Ctrl Pts',(0.23094010767585,0.422726435625391,0.4));
#10586=CARTESIAN_POINT('',(0.23094010767585,0.422726435625391,-0.4));
#10587=CARTESIAN_POINT('Ctrl Pts',(0.23094010767585,0.422726435625391,-0.4));
#10588=CARTESIAN_POINT('Ctrl Pts',(0.346410161513775,0.489393102292058,
-0.2));
#10589=CARTESIAN_POINT('Ctrl Pts',(0.461880215351701,0.422726435625391,
0.));
#10590=CARTESIAN_POINT('',(-0.23094010767585,0.422726435625391,-0.4));
#10591=CARTESIAN_POINT('Ctrl Pts',(-0.23094010767585,0.422726435625391,
-0.4));
#10592=CARTESIAN_POINT('Ctrl Pts',(-5.55111512312578E-17,0.489393102292058,
-0.4));
#10593=CARTESIAN_POINT('Ctrl Pts',(0.23094010767585,0.422726435625391,-0.4));
#10594=CARTESIAN_POINT('Ctrl Pts',(-0.461880215351701,0.422726435625391,
-5.6564012731995E-17));
#10595=CARTESIAN_POINT('Ctrl Pts',(-0.346410161513776,0.489393102292058,
-0.2));
#10596=CARTESIAN_POINT('Ctrl Pts',(-0.23094010767585,0.422726435625391,
-0.4));
#10597=CARTESIAN_POINT('Origin',(0.23094010767585,0.,-0.4));
#10598=CARTESIAN_POINT('',(-0.23094010767585,0.,-0.4));
#10599=CARTESIAN_POINT('',(0.23094010767585,0.,-0.4));
#10600=CARTESIAN_POINT('Origin',(-0.23094010767585,0.,-0.4));
#10601=CARTESIAN_POINT('',(-0.461880215351701,0.,-5.6564012731995E-17));
#10602=CARTESIAN_POINT('Origin',(-0.461880215351701,0.,-5.6564012731995E-17));
#10603=CARTESIAN_POINT('',(-0.230940107675851,0.,0.4));
#10604=CARTESIAN_POINT('Origin',(0.,0.,0.));
#10605=CARTESIAN_POINT('',(-0.2117,0.47,2.59257727379495E-17));
#10606=CARTESIAN_POINT('Origin',(0.,0.47,0.));
#10607=CARTESIAN_POINT('',(-0.2117,0.,2.59257727379495E-17));
#10608=CARTESIAN_POINT('',(-0.2117,0.,2.59257727379495E-17));
#10609=CARTESIAN_POINT('Origin',(0.,0.,0.));
#10610=CARTESIAN_POINT('Origin',(-0.230940107675851,0.,0.4));
#10611=CARTESIAN_POINT('',(0.23094010767585,0.,0.4));
#10612=CARTESIAN_POINT('Origin',(0.461880215351701,0.,0.));
#10613=CARTESIAN_POINT('',(0.461880215351701,0.,0.));
#10614=CARTESIAN_POINT('Origin',(0.23094010767585,0.,0.4));
#10615=CARTESIAN_POINT('Origin',(0.,0.47,0.));
#10616=CARTESIAN_POINT('Origin',(0.,0.,0.));
#10617=CARTESIAN_POINT('',(0.,0.,0.));
#10618=CARTESIAN_POINT('Origin',(0.3,0.4,0.));
#10619=CARTESIAN_POINT('',(-0.3,0.4,-3.67394039744206E-17));
#10620=CARTESIAN_POINT('Origin',(0.,0.4,0.));
#10621=CARTESIAN_POINT('Origin',(0.,0.375,0.));
#10622=CARTESIAN_POINT('',(-0.35,0.35,-4.28626379701573E-17));
#10623=CARTESIAN_POINT('Origin',(0.,0.35,0.));
#10624=CARTESIAN_POINT('',(-0.325,0.375,-3.9801020972289E-17));
#10625=CARTESIAN_POINT('Origin',(0.,0.19,0.));
#10626=CARTESIAN_POINT('',(-0.35,0.03,-4.28626379701574E-17));
#10627=CARTESIAN_POINT('Origin',(0.,0.03,0.));
#10628=CARTESIAN_POINT('',(-0.35,0.19,-4.28626379701574E-17));
#10629=CARTESIAN_POINT('Origin',(0.,0.0149999999999999,0.));
#10630=CARTESIAN_POINT('',(-0.32,-3.29597460435593E-17,-3.91886975727153E-17));
#10631=CARTESIAN_POINT('Origin',(0.,0.,0.));
#10632=CARTESIAN_POINT('',(-0.335,0.0149999999999999,-4.10256677714363E-17));
#10633=CARTESIAN_POINT('Origin',(0.22,0.,0.));
#10634=CARTESIAN_POINT('',(-0.22,-6.93889390390723E-18,-2.69422295812418E-17));
#10635=CARTESIAN_POINT('Origin',(0.,0.,0.));
#10636=CARTESIAN_POINT('Origin',(0.,-0.02,0.));
#10637=CARTESIAN_POINT('',(-0.1954,-0.0492,2.39295984553393E-17));
#10638=CARTESIAN_POINT('Origin',(0.,-0.0492,0.));
#10639=CARTESIAN_POINT('',(-0.21,-0.02,-2.57175827820944E-17));
#10640=CARTESIAN_POINT('Origin',(0.,-0.8,0.));
#10641=CARTESIAN_POINT('',(-0.1954,-1.5646,2.39295984553393E-17));
#10642=CARTESIAN_POINT('Origin',(0.,-1.5646,0.));
#10643=CARTESIAN_POINT('',(-0.1954,-0.8,-2.39295984553393E-17));
#10644=CARTESIAN_POINT('Origin',(0.,-1.58,0.));
#10645=CARTESIAN_POINT('',(-0.16,-1.6,-1.95943487863577E-17));
#10646=CARTESIAN_POINT('Origin',(0.,-1.6,0.));
#10647=CARTESIAN_POINT('',(-0.18,-1.58,-2.20436423846524E-17));
#10648=CARTESIAN_POINT('Origin',(0.,-1.6,0.));
#10649=CARTESIAN_POINT('Origin',(0.0866025403784439,-0.4,-0.15));
#10650=CARTESIAN_POINT('',(0.173205080756888,-0.4,0.));
#10651=CARTESIAN_POINT('',(0.0866025403784439,-0.4,-0.15));
#10652=CARTESIAN_POINT('',(0.173205080756888,-0.4,0.));
#10653=CARTESIAN_POINT('',(0.0866025403784439,-0.64,-0.15));
#10654=CARTESIAN_POINT('',(0.0866025403784439,-0.4,-0.15));
#10655=CARTESIAN_POINT('',(0.173205080756888,-0.64,0.));
#10656=CARTESIAN_POINT('',(0.173205080756888,-0.64,0.));
#10657=CARTESIAN_POINT('',(0.173205080756888,-0.4,0.));
#10658=CARTESIAN_POINT('Origin',(-0.0866025403784438,-0.4,-0.15));
#10659=CARTESIAN_POINT('',(-0.0866025403784438,-0.4,-0.15));
#10660=CARTESIAN_POINT('',(0.0866025403784439,-0.4,-0.15));
#10661=CARTESIAN_POINT('',(-0.0866025403784438,-0.64,-0.15));
#10662=CARTESIAN_POINT('',(-0.0866025403784438,-0.4,-0.15));
#10663=CARTESIAN_POINT('',(0.0866025403784439,-0.64,-0.15));
#10664=CARTESIAN_POINT('Origin',(-0.173205080756888,-0.4,-2.77555756156289E-17));
#10665=CARTESIAN_POINT('',(-0.173205080756888,-0.4,-2.12115047744981E-17));
#10666=CARTESIAN_POINT('',(-0.0866025403784438,-0.4,-0.15));
#10667=CARTESIAN_POINT('',(-0.173205080756888,-0.64,-2.77555756156289E-17));
#10668=CARTESIAN_POINT('',(-0.173205080756888,-0.4,-2.12115047744981E-17));
#10669=CARTESIAN_POINT('',(-0.0866025403784438,-0.64,-0.15));
#10670=CARTESIAN_POINT('Origin',(-0.0866025403784439,-0.4,0.15));
#10671=CARTESIAN_POINT('',(-0.0866025403784439,-0.4,0.15));
#10672=CARTESIAN_POINT('',(-0.173205080756888,-0.4,-2.12115047744981E-17));
#10673=CARTESIAN_POINT('',(-0.0866025403784439,-0.64,0.15));
#10674=CARTESIAN_POINT('',(-0.0866025403784439,-0.4,0.15));
#10675=CARTESIAN_POINT('',(-0.173205080756888,-0.64,-2.12115047744981E-17));
#10676=CARTESIAN_POINT('Origin',(0.0866025403784439,-0.4,0.15));
#10677=CARTESIAN_POINT('',(0.0866025403784439,-0.4,0.15));
#10678=CARTESIAN_POINT('',(-0.0866025403784439,-0.4,0.15));
#10679=CARTESIAN_POINT('',(0.0866025403784439,-0.64,0.15));
#10680=CARTESIAN_POINT('',(0.0866025403784439,-0.4,0.15));
#10681=CARTESIAN_POINT('',(-0.0866025403784439,-0.64,0.15));
#10682=CARTESIAN_POINT('Origin',(0.173205080756888,-0.4,0.));
#10683=CARTESIAN_POINT('',(0.0866025403784439,-0.4,0.15));
#10684=CARTESIAN_POINT('',(0.0866025403784439,-0.64,0.15));
#10685=CARTESIAN_POINT('Origin',(0.,-0.4,-2.77555756156289E-17));
#10686=CARTESIAN_POINT('Origin',(0.,-0.64,-2.77555756156289E-17));
#10687=CARTESIAN_POINT('',(0.,0.,0.));
#10688=CARTESIAN_POINT('',(0.,0.,0.));
#10689=CARTESIAN_POINT('Origin',(7.76256313292354,-1.23743686707646,4.9));
#10690=CARTESIAN_POINT('',(7.59756313292354,-1.23743686707646,5.));
#10691=CARTESIAN_POINT('Origin',(7.76256313292354,-1.23743686707646,5.));
#10692=CARTESIAN_POINT('',(7.59756313292354,-1.23743686707646,6.));
#10693=CARTESIAN_POINT('',(7.59756313292354,-1.23743686707646,4.9));
#10694=CARTESIAN_POINT('Origin',(7.76256313292354,-1.23743686707646,6.));
#10695=CARTESIAN_POINT('Origin',(7.76256313292354,1.23743686707646,4.9));
#10696=CARTESIAN_POINT('',(7.59756313292354,1.23743686707646,5.));
#10697=CARTESIAN_POINT('Origin',(7.76256313292354,1.23743686707646,5.));
#10698=CARTESIAN_POINT('',(7.59756313292354,1.23743686707646,6.));
#10699=CARTESIAN_POINT('',(7.59756313292354,1.23743686707646,4.9));
#10700=CARTESIAN_POINT('Origin',(7.76256313292354,1.23743686707646,6.));
#10701=CARTESIAN_POINT('Origin',(10.2374368670765,1.23743686707646,4.9));
#10702=CARTESIAN_POINT('',(10.0724368670765,1.23743686707646,5.));
#10703=CARTESIAN_POINT('Origin',(10.2374368670765,1.23743686707646,5.));
#10704=CARTESIAN_POINT('',(10.0724368670765,1.23743686707646,6.));
#10705=CARTESIAN_POINT('',(10.0724368670765,1.23743686707646,4.9));
#10706=CARTESIAN_POINT('Origin',(10.2374368670765,1.23743686707646,6.));
#10707=CARTESIAN_POINT('Origin',(10.2374368670765,-1.23743686707646,4.9));
#10708=CARTESIAN_POINT('',(10.0724368670765,-1.23743686707646,5.));
#10709=CARTESIAN_POINT('Origin',(10.2374368670765,-1.23743686707646,5.));
#10710=CARTESIAN_POINT('',(10.0724368670765,-1.23743686707646,6.));
#10711=CARTESIAN_POINT('',(10.0724368670765,-1.23743686707646,4.9));
#10712=CARTESIAN_POINT('Origin',(10.2374368670765,-1.23743686707646,6.));
#10713=CARTESIAN_POINT('Origin',(-1.23743686707646,-1.23743686707646,4.9));
#10714=CARTESIAN_POINT('',(-1.40243686707646,-1.23743686707646,5.));
#10715=CARTESIAN_POINT('Origin',(-1.23743686707646,-1.23743686707646,5.));
#10716=CARTESIAN_POINT('',(-1.40243686707646,-1.23743686707646,6.));
#10717=CARTESIAN_POINT('',(-1.40243686707646,-1.23743686707646,4.9));
#10718=CARTESIAN_POINT('Origin',(-1.23743686707646,-1.23743686707646,6.));
#10719=CARTESIAN_POINT('Origin',(-1.23743686707646,1.23743686707646,4.9));
#10720=CARTESIAN_POINT('',(-1.40243686707646,1.23743686707646,5.));
#10721=CARTESIAN_POINT('Origin',(-1.23743686707646,1.23743686707646,5.));
#10722=CARTESIAN_POINT('',(-1.40243686707646,1.23743686707646,6.));
#10723=CARTESIAN_POINT('',(-1.40243686707646,1.23743686707646,4.9));
#10724=CARTESIAN_POINT('Origin',(-1.23743686707646,1.23743686707646,6.));
#10725=CARTESIAN_POINT('Origin',(1.23743686707646,1.23743686707646,4.9));
#10726=CARTESIAN_POINT('',(1.07243686707646,1.23743686707646,5.));
#10727=CARTESIAN_POINT('Origin',(1.23743686707646,1.23743686707646,5.));
#10728=CARTESIAN_POINT('',(1.07243686707646,1.23743686707646,6.));
#10729=CARTESIAN_POINT('',(1.07243686707646,1.23743686707646,4.9));
#10730=CARTESIAN_POINT('Origin',(1.23743686707646,1.23743686707646,6.));
#10731=CARTESIAN_POINT('Origin',(1.23743686707646,-1.23743686707646,4.9));
#10732=CARTESIAN_POINT('',(1.07243686707646,-1.23743686707646,5.));
#10733=CARTESIAN_POINT('Origin',(1.23743686707646,-1.23743686707646,5.));
#10734=CARTESIAN_POINT('',(1.07243686707646,-1.23743686707646,6.));
#10735=CARTESIAN_POINT('',(1.07243686707646,-1.23743686707646,4.9));
#10736=CARTESIAN_POINT('Origin',(1.23743686707646,-1.23743686707646,6.));
#10737=CARTESIAN_POINT('Origin',(0.,0.,4.9));
#10738=CARTESIAN_POINT('',(-1.5,-1.83697019872103E-16,5.));
#10739=CARTESIAN_POINT('Origin',(0.,0.,5.));
#10740=CARTESIAN_POINT('',(-1.5,1.83697019872103E-16,6.));
#10741=CARTESIAN_POINT('',(-1.5,-1.83697019872103E-16,4.9));
#10742=CARTESIAN_POINT('Origin',(0.,0.,6.));
#10743=CARTESIAN_POINT('Origin',(9.,0.,4.9));
#10744=CARTESIAN_POINT('',(7.5,-1.83697019872103E-16,5.));
#10745=CARTESIAN_POINT('Origin',(9.,0.,5.));
#10746=CARTESIAN_POINT('',(7.5,1.83697019872103E-16,6.));
#10747=CARTESIAN_POINT('',(7.5,-1.83697019872103E-16,4.9));
#10748=CARTESIAN_POINT('Origin',(9.,0.,6.));
#10749=CARTESIAN_POINT('Origin',(9.,0.,5.));
#10750=CARTESIAN_POINT('',(7.16696972201766,0.8,6.));
#10751=CARTESIAN_POINT('',(7.16696972201766,0.8,5.));
#10752=CARTESIAN_POINT('',(7.16696972201766,0.8,5.));
#10753=CARTESIAN_POINT('',(7.16696972201766,-0.8,6.));
#10754=CARTESIAN_POINT('Origin',(9.,0.,6.));
#10755=CARTESIAN_POINT('',(7.16696972201766,-0.8,5.));
#10756=CARTESIAN_POINT('',(7.16696972201766,-0.8,5.));
#10757=CARTESIAN_POINT('Origin',(9.,0.,5.));
#10758=CARTESIAN_POINT('Origin',(9.,0.8,5.));
#10759=CARTESIAN_POINT('',(1.83303027798234,0.8,5.));
#10760=CARTESIAN_POINT('',(9.,0.8,5.));
#10761=CARTESIAN_POINT('',(1.83303027798234,0.8,6.));
#10762=CARTESIAN_POINT('',(1.83303027798234,0.8,5.));
#10763=CARTESIAN_POINT('',(9.,0.8,6.));
#10764=CARTESIAN_POINT('Origin',(0.,0.,5.));
#10765=CARTESIAN_POINT('',(1.83303027798234,-0.8,5.));
#10766=CARTESIAN_POINT('',(0.,-0.8,5.));
#10767=CARTESIAN_POINT('Origin',(0.,0.,5.));
#10768=CARTESIAN_POINT('Origin',(0.,-0.8,5.));
#10769=CARTESIAN_POINT('',(1.83303027798234,-0.8,6.));
#10770=CARTESIAN_POINT('',(0.,-0.8,6.));
#10771=CARTESIAN_POINT('',(1.83303027798234,-0.8,5.));
#10772=CARTESIAN_POINT('Origin',(0.,0.,5.));
#10773=CARTESIAN_POINT('Origin',(0.,0.,6.));
#10774=CARTESIAN_POINT('Origin',(0.,0.,6.));
#10775=CARTESIAN_POINT('',(0.,0.,0.));
#10776=CARTESIAN_POINT('Origin',(-1.23743686707646,-1.23743686707646,4.6));
#10777=CARTESIAN_POINT('',(-1.46243686707646,-1.23743686707646,4.7));
#10778=CARTESIAN_POINT('Origin',(-1.23743686707646,-1.23743686707646,4.7));
#10779=CARTESIAN_POINT('',(-1.46243686707646,-1.23743686707646,5.));
#10780=CARTESIAN_POINT('',(-1.46243686707646,-1.23743686707646,4.6));
#10781=CARTESIAN_POINT('Origin',(-1.23743686707646,-1.23743686707646,5.));
#10782=CARTESIAN_POINT('Origin',(-1.23743686707646,1.23743686707646,4.6));
#10783=CARTESIAN_POINT('',(-1.46243686707646,1.23743686707646,4.7));
#10784=CARTESIAN_POINT('Origin',(-1.23743686707646,1.23743686707646,4.7));
#10785=CARTESIAN_POINT('',(-1.46243686707646,1.23743686707646,5.));
#10786=CARTESIAN_POINT('',(-1.46243686707646,1.23743686707646,4.6));
#10787=CARTESIAN_POINT('Origin',(-1.23743686707646,1.23743686707646,5.));
#10788=CARTESIAN_POINT('Origin',(1.23743686707646,1.23743686707646,4.6));
#10789=CARTESIAN_POINT('',(1.01243686707646,1.23743686707646,4.7));
#10790=CARTESIAN_POINT('Origin',(1.23743686707646,1.23743686707646,4.7));
#10791=CARTESIAN_POINT('',(1.01243686707646,1.23743686707646,5.));
#10792=CARTESIAN_POINT('',(1.01243686707646,1.23743686707646,4.6));
#10793=CARTESIAN_POINT('Origin',(1.23743686707646,1.23743686707646,5.));
#10794=CARTESIAN_POINT('Origin',(1.23743686707646,-1.23743686707646,4.6));
#10795=CARTESIAN_POINT('',(1.01243686707646,-1.23743686707646,4.7));
#10796=CARTESIAN_POINT('Origin',(1.23743686707646,-1.23743686707646,4.7));
#10797=CARTESIAN_POINT('',(1.01243686707646,-1.23743686707646,5.));
#10798=CARTESIAN_POINT('',(1.01243686707646,-1.23743686707646,4.6));
#10799=CARTESIAN_POINT('Origin',(1.23743686707646,-1.23743686707646,5.));
#10800=CARTESIAN_POINT('Origin',(0.,0.,5.));
#10801=CARTESIAN_POINT('',(-1.49,-1.82472373072956E-16,5.05));
#10802=CARTESIAN_POINT('Origin',(0.,0.,5.05));
#10803=CARTESIAN_POINT('',(-1.49,-1.82472373072956E-16,5.));
#10804=CARTESIAN_POINT('',(-1.49,-1.82472373072956E-16,5.));
#10805=CARTESIAN_POINT('Origin',(0.,0.,5.));
#10806=CARTESIAN_POINT('Origin',(0.,0.,5.05));
#10807=CARTESIAN_POINT('',(-1.02,-1.2491397351303E-16,5.05));
#10808=CARTESIAN_POINT('Origin',(0.,0.,5.05));
#10809=CARTESIAN_POINT('Origin',(0.,0.,4.7));
#10810=CARTESIAN_POINT('',(-1.02,-1.2491397351303E-16,4.7));
#10811=CARTESIAN_POINT('',(-1.02,-1.2491397351303E-16,4.7));
#10812=CARTESIAN_POINT('Origin',(0.,0.,4.7));
#10813=CARTESIAN_POINT('Origin',(0.,0.,4.7));
#10814=CARTESIAN_POINT('',(-2.,-2.44929359829471E-16,5.));
#10815=CARTESIAN_POINT('Origin',(0.,0.,5.));
#10816=CARTESIAN_POINT('',(-2.,-2.44929359829471E-16,4.7));
#10817=CARTESIAN_POINT('',(-2.,-2.44929359829471E-16,4.7));
#10818=CARTESIAN_POINT('Origin',(0.,0.,4.7));
#10819=CARTESIAN_POINT('Origin',(0.,0.,5.));
#10820=CARTESIAN_POINT('Origin',(0.,0.,4.7));
#10821=CARTESIAN_POINT('',(0.,0.,0.));
#10822=CARTESIAN_POINT('Origin',(-1.23743686707646,-1.23743686707646,5.9));
#10823=CARTESIAN_POINT('',(-1.46243686707646,-1.23743686707646,6.));
#10824=CARTESIAN_POINT('Origin',(-1.23743686707646,-1.23743686707646,6.));
#10825=CARTESIAN_POINT('',(-1.46243686707646,-1.23743686707646,6.3));
#10826=CARTESIAN_POINT('',(-1.46243686707646,-1.23743686707646,5.9));
#10827=CARTESIAN_POINT('Origin',(-1.23743686707646,-1.23743686707646,6.3));
#10828=CARTESIAN_POINT('Origin',(-1.23743686707646,1.23743686707646,5.9));
#10829=CARTESIAN_POINT('',(-1.46243686707646,1.23743686707646,6.));
#10830=CARTESIAN_POINT('Origin',(-1.23743686707646,1.23743686707646,6.));
#10831=CARTESIAN_POINT('',(-1.46243686707646,1.23743686707646,6.3));
#10832=CARTESIAN_POINT('',(-1.46243686707646,1.23743686707646,5.9));
#10833=CARTESIAN_POINT('Origin',(-1.23743686707646,1.23743686707646,6.3));
#10834=CARTESIAN_POINT('Origin',(1.23743686707646,1.23743686707646,5.9));
#10835=CARTESIAN_POINT('',(1.01243686707646,1.23743686707646,6.));
#10836=CARTESIAN_POINT('Origin',(1.23743686707646,1.23743686707646,6.));
#10837=CARTESIAN_POINT('',(1.01243686707646,1.23743686707646,6.3));
#10838=CARTESIAN_POINT('',(1.01243686707646,1.23743686707646,5.9));
#10839=CARTESIAN_POINT('Origin',(1.23743686707646,1.23743686707646,6.3));
#10840=CARTESIAN_POINT('Origin',(1.23743686707646,-1.23743686707646,5.9));
#10841=CARTESIAN_POINT('',(1.01243686707646,-1.23743686707646,6.));
#10842=CARTESIAN_POINT('Origin',(1.23743686707646,-1.23743686707646,6.));
#10843=CARTESIAN_POINT('',(1.01243686707646,-1.23743686707646,6.3));
#10844=CARTESIAN_POINT('',(1.01243686707646,-1.23743686707646,5.9));
#10845=CARTESIAN_POINT('Origin',(1.23743686707646,-1.23743686707646,6.3));
#10846=CARTESIAN_POINT('Origin',(0.,0.,5.95));
#10847=CARTESIAN_POINT('',(-1.49,-1.82472373072956E-16,6.));
#10848=CARTESIAN_POINT('Origin',(0.,0.,6.));
#10849=CARTESIAN_POINT('',(-1.49,-1.82472373072956E-16,5.95));
#10850=CARTESIAN_POINT('',(-1.49,-1.82472373072956E-16,5.95));
#10851=CARTESIAN_POINT('Origin',(0.,0.,5.95));
#10852=CARTESIAN_POINT('Origin',(0.,0.,5.95));
#10853=CARTESIAN_POINT('',(-1.02,-1.2491397351303E-16,5.95));
#10854=CARTESIAN_POINT('Origin',(0.,0.,5.95));
#10855=CARTESIAN_POINT('Origin',(0.,0.,6.));
#10856=CARTESIAN_POINT('',(-1.02,-1.2491397351303E-16,6.3));
#10857=CARTESIAN_POINT('Origin',(0.,0.,6.3));
#10858=CARTESIAN_POINT('',(-1.02,-1.2491397351303E-16,6.));
#10859=CARTESIAN_POINT('Origin',(0.,0.,6.));
#10860=CARTESIAN_POINT('',(-2.,-2.44929359829471E-16,6.3));
#10861=CARTESIAN_POINT('Origin',(0.,0.,6.3));
#10862=CARTESIAN_POINT('',(-2.,-2.44929359829471E-16,6.));
#10863=CARTESIAN_POINT('',(-2.,-2.44929359829471E-16,6.));
#10864=CARTESIAN_POINT('Origin',(0.,0.,6.));
#10865=CARTESIAN_POINT('Origin',(0.,0.,6.3));
#10866=CARTESIAN_POINT('Origin',(0.,0.,6.));
#10867=CARTESIAN_POINT('',(0.,0.,0.));
#10868=CARTESIAN_POINT('Origin',(7.76256313292354,-1.23743686707646,4.6));
#10869=CARTESIAN_POINT('',(7.53756313292354,-1.23743686707646,4.7));
#10870=CARTESIAN_POINT('Origin',(7.76256313292354,-1.23743686707646,4.7));
#10871=CARTESIAN_POINT('',(7.53756313292354,-1.23743686707646,5.));
#10872=CARTESIAN_POINT('',(7.53756313292354,-1.23743686707646,4.6));
#10873=CARTESIAN_POINT('Origin',(7.76256313292354,-1.23743686707646,5.));
#10874=CARTESIAN_POINT('Origin',(7.76256313292354,1.23743686707646,4.6));
#10875=CARTESIAN_POINT('',(7.53756313292354,1.23743686707646,4.7));
#10876=CARTESIAN_POINT('Origin',(7.76256313292354,1.23743686707646,4.7));
#10877=CARTESIAN_POINT('',(7.53756313292354,1.23743686707646,5.));
#10878=CARTESIAN_POINT('',(7.53756313292354,1.23743686707646,4.6));
#10879=CARTESIAN_POINT('Origin',(7.76256313292354,1.23743686707646,5.));
#10880=CARTESIAN_POINT('Origin',(10.2374368670765,1.23743686707646,4.6));
#10881=CARTESIAN_POINT('',(10.0124368670765,1.23743686707646,4.7));
#10882=CARTESIAN_POINT('Origin',(10.2374368670765,1.23743686707646,4.7));
#10883=CARTESIAN_POINT('',(10.0124368670765,1.23743686707646,5.));
#10884=CARTESIAN_POINT('',(10.0124368670765,1.23743686707646,4.6));
#10885=CARTESIAN_POINT('Origin',(10.2374368670765,1.23743686707646,5.));
#10886=CARTESIAN_POINT('Origin',(10.2374368670765,-1.23743686707646,4.6));
#10887=CARTESIAN_POINT('',(10.0124368670765,-1.23743686707646,4.7));
#10888=CARTESIAN_POINT('Origin',(10.2374368670765,-1.23743686707646,4.7));
#10889=CARTESIAN_POINT('',(10.0124368670765,-1.23743686707646,5.));
#10890=CARTESIAN_POINT('',(10.0124368670765,-1.23743686707646,4.6));
#10891=CARTESIAN_POINT('Origin',(10.2374368670765,-1.23743686707646,5.));
#10892=CARTESIAN_POINT('Origin',(9.,0.,5.));
#10893=CARTESIAN_POINT('',(7.51,-1.82472373072956E-16,5.05));
#10894=CARTESIAN_POINT('Origin',(9.,0.,5.05));
#10895=CARTESIAN_POINT('',(7.51,-1.82472373072956E-16,5.));
#10896=CARTESIAN_POINT('',(7.51,-1.82472373072956E-16,5.));
#10897=CARTESIAN_POINT('Origin',(9.,0.,5.));
#10898=CARTESIAN_POINT('Origin',(9.,0.,5.05));
#10899=CARTESIAN_POINT('',(7.98,-1.2491397351303E-16,5.05));
#10900=CARTESIAN_POINT('Origin',(9.,0.,5.05));
#10901=CARTESIAN_POINT('Origin',(9.,0.,4.7));
#10902=CARTESIAN_POINT('',(7.98,-1.2491397351303E-16,4.7));
#10903=CARTESIAN_POINT('',(7.98,-1.2491397351303E-16,4.7));
#10904=CARTESIAN_POINT('Origin',(9.,0.,4.7));
#10905=CARTESIAN_POINT('Origin',(9.,0.,4.7));
#10906=CARTESIAN_POINT('',(7.,-2.44929359829471E-16,5.));
#10907=CARTESIAN_POINT('Origin',(9.,0.,5.));
#10908=CARTESIAN_POINT('',(7.,-2.44929359829471E-16,4.7));
#10909=CARTESIAN_POINT('',(7.,-2.44929359829471E-16,4.7));
#10910=CARTESIAN_POINT('Origin',(9.,0.,4.7));
#10911=CARTESIAN_POINT('Origin',(9.,0.,5.));
#10912=CARTESIAN_POINT('Origin',(9.,0.,4.7));
#10913=CARTESIAN_POINT('',(0.,0.,0.));
#10914=CARTESIAN_POINT('Origin',(7.76256313292354,-1.23743686707646,5.9));
#10915=CARTESIAN_POINT('',(7.53756313292354,-1.23743686707646,6.));
#10916=CARTESIAN_POINT('Origin',(7.76256313292354,-1.23743686707646,6.));
#10917=CARTESIAN_POINT('',(7.53756313292354,-1.23743686707646,6.3));
#10918=CARTESIAN_POINT('',(7.53756313292354,-1.23743686707646,5.9));
#10919=CARTESIAN_POINT('Origin',(7.76256313292354,-1.23743686707646,6.3));
#10920=CARTESIAN_POINT('Origin',(7.76256313292354,1.23743686707646,5.9));
#10921=CARTESIAN_POINT('',(7.53756313292354,1.23743686707646,6.));
#10922=CARTESIAN_POINT('Origin',(7.76256313292354,1.23743686707646,6.));
#10923=CARTESIAN_POINT('',(7.53756313292354,1.23743686707646,6.3));
#10924=CARTESIAN_POINT('',(7.53756313292354,1.23743686707646,5.9));
#10925=CARTESIAN_POINT('Origin',(7.76256313292354,1.23743686707646,6.3));
#10926=CARTESIAN_POINT('Origin',(10.2374368670765,1.23743686707646,5.9));
#10927=CARTESIAN_POINT('',(10.0124368670765,1.23743686707646,6.));
#10928=CARTESIAN_POINT('Origin',(10.2374368670765,1.23743686707646,6.));
#10929=CARTESIAN_POINT('',(10.0124368670765,1.23743686707646,6.3));
#10930=CARTESIAN_POINT('',(10.0124368670765,1.23743686707646,5.9));
#10931=CARTESIAN_POINT('Origin',(10.2374368670765,1.23743686707646,6.3));
#10932=CARTESIAN_POINT('Origin',(10.2374368670765,-1.23743686707646,5.9));
#10933=CARTESIAN_POINT('',(10.0124368670765,-1.23743686707646,6.));
#10934=CARTESIAN_POINT('Origin',(10.2374368670765,-1.23743686707646,6.));
#10935=CARTESIAN_POINT('',(10.0124368670765,-1.23743686707646,6.3));
#10936=CARTESIAN_POINT('',(10.0124368670765,-1.23743686707646,5.9));
#10937=CARTESIAN_POINT('Origin',(10.2374368670765,-1.23743686707646,6.3));
#10938=CARTESIAN_POINT('Origin',(9.,0.,5.95));
#10939=CARTESIAN_POINT('',(7.51,-1.82472373072956E-16,6.));
#10940=CARTESIAN_POINT('Origin',(9.,0.,6.));
#10941=CARTESIAN_POINT('',(7.51,-1.82472373072956E-16,5.95));
#10942=CARTESIAN_POINT('',(7.51,-1.82472373072956E-16,5.95));
#10943=CARTESIAN_POINT('Origin',(9.,0.,5.95));
#10944=CARTESIAN_POINT('Origin',(9.,0.,5.95));
#10945=CARTESIAN_POINT('',(7.98,-1.2491397351303E-16,5.95));
#10946=CARTESIAN_POINT('Origin',(9.,0.,5.95));
#10947=CARTESIAN_POINT('Origin',(9.,0.,6.));
#10948=CARTESIAN_POINT('',(7.98,-1.2491397351303E-16,6.3));
#10949=CARTESIAN_POINT('Origin',(9.,0.,6.3));
#10950=CARTESIAN_POINT('',(7.98,-1.2491397351303E-16,6.));
#10951=CARTESIAN_POINT('Origin',(9.,0.,6.));
#10952=CARTESIAN_POINT('',(7.,-2.44929359829471E-16,6.3));
#10953=CARTESIAN_POINT('Origin',(9.,0.,6.3));
#10954=CARTESIAN_POINT('',(7.,-2.44929359829471E-16,6.));
#10955=CARTESIAN_POINT('',(7.,-2.44929359829471E-16,6.));
#10956=CARTESIAN_POINT('Origin',(9.,0.,6.));
#10957=CARTESIAN_POINT('Origin',(9.,0.,6.3));
#10958=CARTESIAN_POINT('Origin',(9.,0.,6.));
#10959=CARTESIAN_POINT('',(0.,0.,0.));
#10960=CARTESIAN_POINT('Origin',(2.4,2.5,8.05));
#10961=CARTESIAN_POINT('',(2.50492424822054,2.57,8.05));
#10962=CARTESIAN_POINT('',(2.5,2.5,8.12));
#10963=CARTESIAN_POINT('Ctrl Pts',(2.50492424822054,2.57,8.05));
#10964=CARTESIAN_POINT('Ctrl Pts',(2.50492424822054,2.57,8.05880184230815));
#10965=CARTESIAN_POINT('Ctrl Pts',(2.50466528015196,2.56823857908987,8.06818235803024));
#10966=CARTESIAN_POINT('Ctrl Pts',(2.50373308905894,2.56109125434544,8.08542542296838));
#10967=CARTESIAN_POINT('Ctrl Pts',(2.50307367614139,2.5557059746568,8.09328897470932));
#10968=CARTESIAN_POINT('Ctrl Pts',(2.50183839619558,2.54328905662912,8.10570589273699));
#10969=CARTESIAN_POINT('Ctrl Pts',(2.50118181447624,2.53542546943526,8.11109123666712));
#10970=CARTESIAN_POINT('Ctrl Pts',(2.50025611494785,2.51818228380197,8.11823860827541));
#10971=CARTESIAN_POINT('Ctrl Pts',(2.5,2.50880172616976,8.12));
#10972=CARTESIAN_POINT('Ctrl Pts',(2.5,2.5,8.12));
#10973=CARTESIAN_POINT('',(2.5,2.5,7.98));
#10974=CARTESIAN_POINT('Ctrl Pts',(2.5,2.5,7.98));
#10975=CARTESIAN_POINT('Ctrl Pts',(2.5,2.50880172616976,7.98));
#10976=CARTESIAN_POINT('Ctrl Pts',(2.50025611494785,2.51818228380197,7.98176139172459));
#10977=CARTESIAN_POINT('Ctrl Pts',(2.50118181447624,2.53542546943525,7.98890876333288));
#10978=CARTESIAN_POINT('Ctrl Pts',(2.50183839619558,2.54328905662912,7.99429410726301));
#10979=CARTESIAN_POINT('Ctrl Pts',(2.50307367614139,2.5557059746568,8.00671102529068));
#10980=CARTESIAN_POINT('Ctrl Pts',(2.50373308905894,2.56109125434544,8.01457457703162));
#10981=CARTESIAN_POINT('Ctrl Pts',(2.50466528015196,2.56823857908987,8.03181764196976));
#10982=CARTESIAN_POINT('Ctrl Pts',(2.50492424822054,2.57,8.04119815769185));
#10983=CARTESIAN_POINT('Ctrl Pts',(2.50492424822054,2.57,8.05));
#10984=CARTESIAN_POINT('Ctrl Pts',(2.5,2.5,8.12));
#10985=CARTESIAN_POINT('Ctrl Pts',(2.5,2.49119827383024,8.12));
#10986=CARTESIAN_POINT('Ctrl Pts',(2.50025611494785,2.48181771619803,8.11823860827541));
#10987=CARTESIAN_POINT('Ctrl Pts',(2.50118181447624,2.46457453056474,8.11109123666712));
#10988=CARTESIAN_POINT('Ctrl Pts',(2.50183839619558,2.45671094337088,8.10570589273699));
#10989=CARTESIAN_POINT('Ctrl Pts',(2.50307367614139,2.4442940253432,8.09328897470932));
#10990=CARTESIAN_POINT('Ctrl Pts',(2.50373308905894,2.43890874565455,8.08542542296837));
#10991=CARTESIAN_POINT('Ctrl Pts',(2.50466528015196,2.43176142091013,8.06818235803023));
#10992=CARTESIAN_POINT('Ctrl Pts',(2.50492424822054,2.43,8.05880184230815));
#10993=CARTESIAN_POINT('Ctrl Pts',(2.50492424822054,2.43,8.04119815769185));
#10994=CARTESIAN_POINT('Ctrl Pts',(2.50466528015196,2.43176142091014,8.03181764196976));
#10995=CARTESIAN_POINT('Ctrl Pts',(2.50373308905894,2.43890874565456,8.01457457703162));
#10996=CARTESIAN_POINT('Ctrl Pts',(2.50307367614139,2.4442940253432,8.00671102529068));
#10997=CARTESIAN_POINT('Ctrl Pts',(2.50183839619558,2.45671094337088,7.99429410726301));
#10998=CARTESIAN_POINT('Ctrl Pts',(2.50118181447624,2.46457453056474,7.98890876333288));
#10999=CARTESIAN_POINT('Ctrl Pts',(2.50025611494785,2.48181771619803,7.98176139172459));
#11000=CARTESIAN_POINT('Ctrl Pts',(2.5,2.49119827383024,7.98));
#11001=CARTESIAN_POINT('Ctrl Pts',(2.5,2.5,7.98));
#11002=CARTESIAN_POINT('',(3.5,2.5,8.12));
#11003=CARTESIAN_POINT('',(2.4,2.5,8.12));
#11004=CARTESIAN_POINT('',(3.49507575177946,2.57,8.05));
#11005=CARTESIAN_POINT('Ctrl Pts',(3.49507575177946,2.57,8.05));
#11006=CARTESIAN_POINT('Ctrl Pts',(3.49507575177946,2.57,8.04119815769185));
#11007=CARTESIAN_POINT('Ctrl Pts',(3.49533471984804,2.56823857908987,8.03181764196976));
#11008=CARTESIAN_POINT('Ctrl Pts',(3.49626691094106,2.56109125434544,8.01457457703162));
#11009=CARTESIAN_POINT('Ctrl Pts',(3.49692632385861,2.5557059746568,8.00671102529068));
#11010=CARTESIAN_POINT('Ctrl Pts',(3.49816160380442,2.54328905662912,7.99429410726301));
#11011=CARTESIAN_POINT('Ctrl Pts',(3.49881818552376,2.53542546943526,7.98890876333288));
#11012=CARTESIAN_POINT('Ctrl Pts',(3.49974388505215,2.51818228380197,7.98176139172459));
#11013=CARTESIAN_POINT('Ctrl Pts',(3.5,2.50880172616976,7.98));
#11014=CARTESIAN_POINT('Ctrl Pts',(3.5,2.49119827383024,7.98));
#11015=CARTESIAN_POINT('Ctrl Pts',(3.49974388505215,2.48181771619803,7.98176139172459));
#11016=CARTESIAN_POINT('Ctrl Pts',(3.49881818552376,2.46457453056474,7.98890876333288));
#11017=CARTESIAN_POINT('Ctrl Pts',(3.49816160380442,2.45671094337088,7.99429410726301));
#11018=CARTESIAN_POINT('Ctrl Pts',(3.49692632385861,2.4442940253432,8.00671102529068));
#11019=CARTESIAN_POINT('Ctrl Pts',(3.49626691094106,2.43890874565456,8.01457457703162));
#11020=CARTESIAN_POINT('Ctrl Pts',(3.49533471984804,2.43176142091013,8.03181764196976));
#11021=CARTESIAN_POINT('Ctrl Pts',(3.49507575177946,2.43,8.04119815769185));
#11022=CARTESIAN_POINT('Ctrl Pts',(3.49507575177946,2.43,8.05880184230815));
#11023=CARTESIAN_POINT('Ctrl Pts',(3.49533471984804,2.43176142091013,8.06818235803024));
#11024=CARTESIAN_POINT('Ctrl Pts',(3.49626691094106,2.43890874565456,8.08542542296838));
#11025=CARTESIAN_POINT('Ctrl Pts',(3.49692632385861,2.4442940253432,8.09328897470932));
#11026=CARTESIAN_POINT('Ctrl Pts',(3.49816160380442,2.45671094337088,8.10570589273699));
#11027=CARTESIAN_POINT('Ctrl Pts',(3.49881818552376,2.46457453056474,8.11109123666712));
#11028=CARTESIAN_POINT('Ctrl Pts',(3.49974388505215,2.48181771619803,8.11823860827541));
#11029=CARTESIAN_POINT('Ctrl Pts',(3.5,2.49119827383024,8.12));
#11030=CARTESIAN_POINT('Ctrl Pts',(3.5,2.5,8.12));
#11031=CARTESIAN_POINT('Ctrl Pts',(3.5,2.5,8.12));
#11032=CARTESIAN_POINT('Ctrl Pts',(3.5,2.50880172616976,8.12));
#11033=CARTESIAN_POINT('Ctrl Pts',(3.49974388505215,2.51818228380197,8.11823860827541));
#11034=CARTESIAN_POINT('Ctrl Pts',(3.49881818552376,2.53542546943526,8.11109123666712));
#11035=CARTESIAN_POINT('Ctrl Pts',(3.49816160380442,2.54328905662912,8.10570589273699));
#11036=CARTESIAN_POINT('Ctrl Pts',(3.49692632385861,2.5557059746568,8.09328897470932));
#11037=CARTESIAN_POINT('Ctrl Pts',(3.49626691094106,2.56109125434544,8.08542542296838));
#11038=CARTESIAN_POINT('Ctrl Pts',(3.49533471984804,2.56823857908987,8.06818235803024));
#11039=CARTESIAN_POINT('Ctrl Pts',(3.49507575177946,2.57,8.05880184230815));
#11040=CARTESIAN_POINT('Ctrl Pts',(3.49507575177946,2.57,8.05));
#11041=CARTESIAN_POINT('Origin',(3.,2.5,6.4));
#11042=CARTESIAN_POINT('',(2.5,2.5,8.4));
#11043=CARTESIAN_POINT('Origin',(3.,2.5,8.4));
#11044=CARTESIAN_POINT('',(2.5,2.5,6.4));
#11045=CARTESIAN_POINT('',(2.5,2.5,6.4));
#11046=CARTESIAN_POINT('',(2.5,2.5,6.4));
#11047=CARTESIAN_POINT('',(3.5,2.5,6.4));
#11048=CARTESIAN_POINT('Origin',(3.,2.5,6.4));
#11049=CARTESIAN_POINT('',(3.,3.,6.4));
#11050=CARTESIAN_POINT('Origin',(3.,2.5,6.4));
#11051=CARTESIAN_POINT('Origin',(3.,2.5,6.4));
#11052=CARTESIAN_POINT('Origin',(3.,2.5,8.4));
#11053=CARTESIAN_POINT('Origin',(3.,1.5,6.4));
#11054=CARTESIAN_POINT('',(2.5,3.,6.4));
#11055=CARTESIAN_POINT('',(3.5,3.,6.4));
#11056=CARTESIAN_POINT('',(2.5,3.,6.4));
#11057=CARTESIAN_POINT('Origin',(3.,1.5,6.4));
#11058=CARTESIAN_POINT('',(3.5,3.,6.4));
#11059=CARTESIAN_POINT('',(3.5,0.,6.4));
#11060=CARTESIAN_POINT('',(3.5,3.,6.4));
#11061=CARTESIAN_POINT('Origin',(3.,1.5,6.4));
#11062=CARTESIAN_POINT('',(2.5,0.,6.4));
#11063=CARTESIAN_POINT('',(2.5,3.,6.4));
#11064=CARTESIAN_POINT('',(3.5,0.,6.4));
#11065=CARTESIAN_POINT('',(2.5,0.,6.4));
#11066=CARTESIAN_POINT('',(3.5,0.,6.4));
#11067=CARTESIAN_POINT('Origin',(3.5,3.,6.));
#11068=CARTESIAN_POINT('',(3.5,3.,6.));
#11069=CARTESIAN_POINT('',(2.5,3.,6.));
#11070=CARTESIAN_POINT('',(3.5,3.,6.));
#11071=CARTESIAN_POINT('',(2.5,3.,6.));
#11072=CARTESIAN_POINT('',(3.5,3.,6.));
#11073=CARTESIAN_POINT('Origin',(3.5,0.,6.));
#11074=CARTESIAN_POINT('',(3.5,0.,6.));
#11075=CARTESIAN_POINT('',(3.5,0.,6.));
#11076=CARTESIAN_POINT('',(3.5,0.,6.));
#11077=CARTESIAN_POINT('Origin',(2.5,0.,6.));
#11078=CARTESIAN_POINT('',(2.5,0.,6.));
#11079=CARTESIAN_POINT('',(2.5,0.,6.));
#11080=CARTESIAN_POINT('',(2.5,0.,6.));
#11081=CARTESIAN_POINT('Origin',(2.5,3.,6.));
#11082=CARTESIAN_POINT('',(2.5,3.,6.));
#11083=CARTESIAN_POINT('Origin',(3.,1.5,6.));
#11084=CARTESIAN_POINT('',(0.,0.,0.));
#11085=CARTESIAN_POINT('',(0.,0.,0.));
#11086=CARTESIAN_POINT('Origin',(0.,0.,0.));
#11087=CARTESIAN_POINT('',(-0.976185,-0.246528389340863,-1.19548183562566E-16));
#11088=CARTESIAN_POINT('',(-1.19548183562566E-16,-0.246528389340863,0.976185));
#11089=CARTESIAN_POINT('Origin',(0.,-0.246528389340863,0.));
#11090=CARTESIAN_POINT('Origin',(0.,-0.246528389340863,0.));
#11091=CARTESIAN_POINT('',(-1.19548183562566E-16,0.246528389340863,0.976185));
#11092=CARTESIAN_POINT('Origin',(-1.22464679914735E-16,0.,1.));
#11093=CARTESIAN_POINT('',(-0.976185,0.246528389340863,1.19548183562566E-16));
#11094=CARTESIAN_POINT('Origin',(0.,0.246528389340863,0.));
#11095=CARTESIAN_POINT('Origin',(0.,0.246528389340863,0.));
#11096=CARTESIAN_POINT('Origin',(0.,0.,0.));
#11097=CARTESIAN_POINT('',(-0.976185,0.45,-1.19548183562566E-16));
#11098=CARTESIAN_POINT('',(-0.976185,0.,-1.19548183562566E-16));
#11099=CARTESIAN_POINT('Origin',(0.,0.45,0.));
#11100=CARTESIAN_POINT('Origin',(0.,0.,0.));
#11101=CARTESIAN_POINT('',(-0.5,-0.39,-6.12323399573677E-17));
#11102=CARTESIAN_POINT('Origin',(0.,-0.39,0.));
#11103=CARTESIAN_POINT('',(-0.5,0.39,-6.12323399573677E-17));
#11104=CARTESIAN_POINT('',(-0.5,0.,-6.12323399573677E-17));
#11105=CARTESIAN_POINT('Origin',(0.,0.39,0.));
#11106=CARTESIAN_POINT('Origin',(0.,0.42,0.));
#11107=CARTESIAN_POINT('',(-0.56,0.45,-6.85802207522518E-17));
#11108=CARTESIAN_POINT('',(-0.53,0.42,-6.49062803548097E-17));
#11109=CARTESIAN_POINT('Origin',(0.,0.45,0.));
#11110=CARTESIAN_POINT('Origin',(0.976185,0.45,0.));
#11111=CARTESIAN_POINT('Origin',(0.,0.,0.));
#11112=CARTESIAN_POINT('',(-0.976185,-0.45,-1.19548183562566E-16));
#11113=CARTESIAN_POINT('Origin',(0.,-0.45,0.));
#11114=CARTESIAN_POINT('',(-0.976185,0.,-1.19548183562566E-16));
#11115=CARTESIAN_POINT('Origin',(0.56,-0.45,0.));
#11116=CARTESIAN_POINT('',(-0.56,-0.45,-6.85802207522518E-17));
#11117=CARTESIAN_POINT('Origin',(0.,-0.45,0.));
#11118=CARTESIAN_POINT('Origin',(0.,-0.42,0.));
#11119=CARTESIAN_POINT('',(-0.53,-0.42,-6.49062803548097E-17));
#11120=CARTESIAN_POINT('',(0.,0.,0.));
#11121=CARTESIAN_POINT('Origin',(0.,0.,0.));
#11122=CARTESIAN_POINT('',(-1.023815,0.246528389340863,-1.25381176266905E-16));
#11123=CARTESIAN_POINT('',(-1.25381176266905E-16,0.246528389340863,1.023815));
#11124=CARTESIAN_POINT('Origin',(0.,0.246528389340863,0.));
#11125=CARTESIAN_POINT('Origin',(0.,0.246528389340863,0.));
#11126=CARTESIAN_POINT('',(-1.25381176266905E-16,-0.246528389340863,1.023815));
#11127=CARTESIAN_POINT('Origin',(-1.22464679914735E-16,0.,1.));
#11128=CARTESIAN_POINT('',(-1.023815,-0.246528389340863,1.25381176266905E-16));
#11129=CARTESIAN_POINT('Origin',(0.,-0.246528389340863,0.));
#11130=CARTESIAN_POINT('Origin',(0.,-0.246528389340863,0.));
#11131=CARTESIAN_POINT('Origin',(0.,0.,0.));
#11132=CARTESIAN_POINT('',(-1.023815,-0.45,-1.25381176266905E-16));
#11133=CARTESIAN_POINT('Origin',(0.,-0.45,0.));
#11134=CARTESIAN_POINT('',(-1.023815,0.,-1.25381176266905E-16));
#11135=CARTESIAN_POINT('Origin',(1.44,0.45,0.));
#11136=CARTESIAN_POINT('',(-1.44,0.45,-1.76349139077219E-16));
#11137=CARTESIAN_POINT('Origin',(0.,0.45,0.));
#11138=CARTESIAN_POINT('',(-1.023815,0.45,-1.25381176266905E-16));
#11139=CARTESIAN_POINT('Origin',(0.,0.45,0.));
#11140=CARTESIAN_POINT('Origin',(0.,0.42,0.));
#11141=CARTESIAN_POINT('',(-1.5,0.39,-1.83697019872103E-16));
#11142=CARTESIAN_POINT('Origin',(0.,0.39,0.));
#11143=CARTESIAN_POINT('',(-1.47,0.42,-1.80023079474661E-16));
#11144=CARTESIAN_POINT('Origin',(0.,0.,0.));
#11145=CARTESIAN_POINT('',(-1.5,-0.39,-1.83697019872103E-16));
#11146=CARTESIAN_POINT('Origin',(0.,-0.39,0.));
#11147=CARTESIAN_POINT('',(-1.5,0.,-1.83697019872103E-16));
#11148=CARTESIAN_POINT('Origin',(0.,-0.42,0.));
#11149=CARTESIAN_POINT('',(-1.44,-0.45,-1.76349139077219E-16));
#11150=CARTESIAN_POINT('Origin',(0.,-0.45,0.));
#11151=CARTESIAN_POINT('',(-1.47,-0.42,-1.80023079474661E-16));
#11152=CARTESIAN_POINT('Origin',(1.023815,-0.45,0.));
#11153=CARTESIAN_POINT('Origin',(0.,0.,0.));
#11154=CARTESIAN_POINT('',(-1.023815,0.,-1.25381176266905E-16));
#11155=CARTESIAN_POINT('',(0.,0.,0.));
#11156=CARTESIAN_POINT('Origin',(1.,0.,0.));
#11157=CARTESIAN_POINT('',(1.,-1.78583896120461E-33,0.23815));
#11158=CARTESIAN_POINT('',(1.,-1.78583896120461E-33,-0.23815));
#11159=CARTESIAN_POINT('Origin',(1.,0.,0.));
#11160=CARTESIAN_POINT('Origin',(0.707106781186548,0.,-0.707106781186547));
#11161=CARTESIAN_POINT('',(0.875504261126124,-1.78583896120461E-33,-0.538709301246971));
#11162=CARTESIAN_POINT('',(0.538709301246971,-1.78583896120461E-33,-0.875504261126124));
#11163=CARTESIAN_POINT('Origin',(0.707106781186548,0.,-0.707106781186547));
#11164=CARTESIAN_POINT('Origin',(6.12323399573677E-17,0.,-1.));
#11165=CARTESIAN_POINT('',(0.23815,-1.78583896120461E-33,-1.));
#11166=CARTESIAN_POINT('',(-0.23815,-1.78583896120461E-33,-1.));
#11167=CARTESIAN_POINT('Origin',(6.12323399573677E-17,0.,-1.));
#11168=CARTESIAN_POINT('Origin',(-0.707106781186547,0.,-0.707106781186548));
#11169=CARTESIAN_POINT('',(-0.538709301246971,-1.78583896120461E-33,-0.875504261126124));
#11170=CARTESIAN_POINT('',(-0.875504261126124,-1.78583896120461E-33,-0.538709301246971));
#11171=CARTESIAN_POINT('Origin',(-0.707106781186547,0.,-0.707106781186548));
#11172=CARTESIAN_POINT('Origin',(-1.,0.,-1.22464679914735E-16));
#11173=CARTESIAN_POINT('',(-1.,-1.78583896120461E-33,-0.23815));
#11174=CARTESIAN_POINT('',(-1.,-1.78583896120461E-33,0.23815));
#11175=CARTESIAN_POINT('Origin',(-1.,0.,-1.22464679914735E-16));
#11176=CARTESIAN_POINT('Origin',(-0.707106781186548,0.,0.707106781186547));
#11177=CARTESIAN_POINT('',(-0.875504261126124,-7.94881478324376E-33,0.538709301246971));
#11178=CARTESIAN_POINT('',(-0.538709301246971,4.37713686083455E-33,0.875504261126124));
#11179=CARTESIAN_POINT('Origin',(-0.707106781186548,0.,0.707106781186547));
#11180=CARTESIAN_POINT('Origin',(-1.83697019872103E-16,0.,1.));
#11181=CARTESIAN_POINT('',(-0.23815,-1.78583896120461E-33,1.));
#11182=CARTESIAN_POINT('',(0.23815,-1.78583896120461E-33,1.));
#11183=CARTESIAN_POINT('Origin',(-1.83697019872103E-16,0.,1.));
#11184=CARTESIAN_POINT('Origin',(0.707106781186547,0.,0.707106781186548));
#11185=CARTESIAN_POINT('',(0.538709301246971,-4.86732687222419E-33,0.875504261126124));
#11186=CARTESIAN_POINT('',(0.875504261126124,1.29564894981497E-33,0.538709301246971));
#11187=CARTESIAN_POINT('Origin',(0.707106781186547,0.,0.707106781186548));
#11188=CARTESIAN_POINT('',(0.,0.,0.));
#11189=CARTESIAN_POINT('Origin',(0.707106781186547,0.,0.707106781186548));
#11190=CARTESIAN_POINT('',(0.504455939115715,-0.04763,0.841298510752802));
#11191=CARTESIAN_POINT('',(0.841298510752802,-0.04763,0.504455939115715));
#11192=CARTESIAN_POINT('Ctrl Pts',(0.504455939115715,-0.04763,0.841298510752802));
#11193=CARTESIAN_POINT('Ctrl Pts',(0.508899795931835,-0.0740444353928835,
0.838633903678357));
#11194=CARTESIAN_POINT('Ctrl Pts',(0.517157748491652,-0.0999305678883309,
0.833661031856294));
#11195=CARTESIAN_POINT('Ctrl Pts',(0.537715343527944,-0.142345102874864,
0.820511285096538));
#11196=CARTESIAN_POINT('Ctrl Pts',(0.548874290046456,-0.159766064500479,
0.813159949759));
#11197=CARTESIAN_POINT('Ctrl Pts',(0.573915184558107,-0.190326085855194,
0.795684265985089));
#11198=CARTESIAN_POINT('Ctrl Pts',(0.587792702767295,-0.203463743702801,
0.78555112003688));
#11199=CARTESIAN_POINT('Ctrl Pts',(0.615966552324775,-0.224161999508995,
0.763642258217233));
#11200=CARTESIAN_POINT('Ctrl Pts',(0.631684198665438,-0.232861760990032,
0.750785745543687));
#11201=CARTESIAN_POINT('Ctrl Pts',(0.663382628119203,-0.244251601209411,
0.722929908501543));
#11202=CARTESIAN_POINT('Ctrl Pts',(0.679352081686668,-0.246942143572133,
0.707917883896095));
#11203=CARTESIAN_POINT('Ctrl Pts',(0.707917883896095,-0.246942143572133,
0.679352081686668));
#11204=CARTESIAN_POINT('Ctrl Pts',(0.722929908501543,-0.244251601209411,
0.663382628119203));
#11205=CARTESIAN_POINT('Ctrl Pts',(0.750785745543687,-0.232861760990032,
0.631684198665439));
#11206=CARTESIAN_POINT('Ctrl Pts',(0.763642258217232,-0.224161999508995,
0.615966552324775));
#11207=CARTESIAN_POINT('Ctrl Pts',(0.78555112003688,-0.203463743702801,
0.587792702767295));
#11208=CARTESIAN_POINT('Ctrl Pts',(0.795684265985088,-0.190326085855194,
0.573915184558108));
#11209=CARTESIAN_POINT('Ctrl Pts',(0.813159949759,-0.15976606450048,0.548874290046456));
#11210=CARTESIAN_POINT('Ctrl Pts',(0.820511285096538,-0.142345102874864,
0.537715343527944));
#11211=CARTESIAN_POINT('Ctrl Pts',(0.833661031856294,-0.099930567888331,
0.517157748491653));
#11212=CARTESIAN_POINT('Ctrl Pts',(0.838633903678357,-0.0740444353928835,
0.508899795931835));
#11213=CARTESIAN_POINT('Ctrl Pts',(0.841298510752801,-0.0476299999999999,
0.504455939115715));
#11214=CARTESIAN_POINT('',(0.528110872004958,-0.04763,0.871530771444223));
#11215=CARTESIAN_POINT('Origin',(0.707106781186547,-0.04763,0.707106781186548));
#11216=CARTESIAN_POINT('',(0.871530771444223,-0.04763,0.528110872004959));
#11217=CARTESIAN_POINT('Ctrl Pts',(0.871530771444223,-0.0476300000000001,
0.528110872004958));
#11218=CARTESIAN_POINT('Ctrl Pts',(0.87014664509073,-0.0609922781173483,
0.530395067942936));
#11219=CARTESIAN_POINT('Ctrl Pts',(0.868149331745851,-0.0742967091364493,
0.533674141594226));
#11220=CARTESIAN_POINT('Ctrl Pts',(0.85981294420286,-0.115492077056649,
0.54708917182331));
#11221=CARTESIAN_POINT('Ctrl Pts',(0.850993704737257,-0.141695629206859,
0.560922177770136));
#11222=CARTESIAN_POINT('Ctrl Pts',(0.830754510485543,-0.181890537957859,
0.590422647829571));
#11223=CARTESIAN_POINT('Ctrl Pts',(0.816896541396381,-0.201072148666545,
0.609616703125488));
#11224=CARTESIAN_POINT('Ctrl Pts',(0.792310597819928,-0.223955109275652,
0.641117951819998));
#11225=CARTESIAN_POINT('Ctrl Pts',(0.779109323683612,-0.232742381310829,
0.657208095763053));
#11226=CARTESIAN_POINT('Ctrl Pts',(0.750552691816206,-0.244234834628584,
0.68964083160521));
#11227=CARTESIAN_POINT('Ctrl Pts',(0.735185187071673,-0.246942143572133,
0.705971972091755));
#11228=CARTESIAN_POINT('Ctrl Pts',(0.705971972091754,-0.246942143572133,
0.735185187071673));
#11229=CARTESIAN_POINT('Ctrl Pts',(0.689640831605209,-0.244234834628584,
0.750552691816206));
#11230=CARTESIAN_POINT('Ctrl Pts',(0.657208095763052,-0.232742381310829,
0.779109323683612));
#11231=CARTESIAN_POINT('Ctrl Pts',(0.641117951819998,-0.223955109275652,
0.792310597819928));
#11232=CARTESIAN_POINT('Ctrl Pts',(0.609616703125487,-0.201072148666545,
0.816896541396382));
#11233=CARTESIAN_POINT('Ctrl Pts',(0.590422647829571,-0.181890537957858,
0.830754510485544));
#11234=CARTESIAN_POINT('Ctrl Pts',(0.560922177770135,-0.141695629206858,
0.850993704737257));
#11235=CARTESIAN_POINT('Ctrl Pts',(0.547089171823309,-0.115492077056649,
0.859812944202861));
#11236=CARTESIAN_POINT('Ctrl Pts',(0.533674141594226,-0.0742967091364491,
0.868149331745852));
#11237=CARTESIAN_POINT('Ctrl Pts',(0.530395067942936,-0.0609922781173483,
0.870146645090731));
#11238=CARTESIAN_POINT('Ctrl Pts',(0.528110872004958,-0.0476300000000001,
0.871530771444223));
#11239=CARTESIAN_POINT('Origin',(0.707106781186547,-0.04763,0.707106781186548));
#11240=CARTESIAN_POINT('Origin',(0.,-0.166705,0.));
#11241=CARTESIAN_POINT('',(0.242834539687906,-0.04763,0.989696097314));
#11242=CARTESIAN_POINT('Origin',(0.,-0.04763,0.));
#11243=CARTESIAN_POINT('',(-0.242834539687907,-0.04763,0.989696097314));
#11244=CARTESIAN_POINT('Ctrl Pts',(0.242834539687906,-0.04763,0.989696097314));
#11245=CARTESIAN_POINT('Ctrl Pts',(0.24024064412003,-0.0609922781173483,
0.990332542620729));
#11246=CARTESIAN_POINT('Ctrl Pts',(0.236509675094874,-0.0742967091364492,
0.991238884025248));
#11247=CARTESIAN_POINT('Ctrl Pts',(0.221129100087819,-0.115492077056649,
0.994830026707808));
#11248=CARTESIAN_POINT('Ctrl Pts',(0.205111543747588,-0.141695629206859,
0.998375294985966));
#11249=CARTESIAN_POINT('Ctrl Pts',(0.169940289819232,-0.181890537957859,
1.00492400591205));
#11250=CARTESIAN_POINT('Ctrl Pts',(0.1465689792446,-0.201072148666545,1.00869718865384));
#11251=CARTESIAN_POINT('Ctrl Pts',(0.106909345252087,-0.223955109275652,
1.01358704779679));
#11252=CARTESIAN_POINT('Ctrl Pts',(0.0861971848975941,-0.232742381310829,
1.0156297872271));
#11253=CARTESIAN_POINT('Ctrl Pts',(0.0430711894098822,-0.244234834628584,
1.01837060663223));
#11254=CARTESIAN_POINT('Ctrl Pts',(0.0206568624125605,-0.246942143572133,
1.019052));
#11255=CARTESIAN_POINT('Ctrl Pts',(-0.0206568624125608,-0.246942143572133,
1.019052));
#11256=CARTESIAN_POINT('Ctrl Pts',(-0.0430711894098825,-0.244234834628584,
1.01837060663223));
#11257=CARTESIAN_POINT('Ctrl Pts',(-0.0861971848975943,-0.232742381310829,
1.0156297872271));
#11258=CARTESIAN_POINT('Ctrl Pts',(-0.106909345252088,-0.223955109275652,
1.01358704779679));
#11259=CARTESIAN_POINT('Ctrl Pts',(-0.1465689792446,-0.201072148666545,
1.00869718865384));
#11260=CARTESIAN_POINT('Ctrl Pts',(-0.169940289819232,-0.181890537957859,
1.00492400591205));
#11261=CARTESIAN_POINT('Ctrl Pts',(-0.205111543747588,-0.141695629206859,
0.998375294985966));
#11262=CARTESIAN_POINT('Ctrl Pts',(-0.221129100087819,-0.115492077056649,
0.994830026707808));
#11263=CARTESIAN_POINT('Ctrl Pts',(-0.236509675094875,-0.0742967091364493,
0.991238884025248));
#11264=CARTESIAN_POINT('Ctrl Pts',(-0.24024064412003,-0.0609922781173483,
0.990332542620729));
#11265=CARTESIAN_POINT('Ctrl Pts',(-0.242834539687907,-0.04763,0.989696097314));
#11266=CARTESIAN_POINT('',(-0.528110872004959,-0.04763,0.871530771444223));
#11267=CARTESIAN_POINT('Origin',(0.,-0.04763,0.));
#11268=CARTESIAN_POINT('',(-0.871530771444223,-0.04763,0.528110872004958));
#11269=CARTESIAN_POINT('Ctrl Pts',(-0.528110872004958,-0.0476300000000001,
0.871530771444223));
#11270=CARTESIAN_POINT('Ctrl Pts',(-0.530395067942936,-0.0609922781173484,
0.87014664509073));
#11271=CARTESIAN_POINT('Ctrl Pts',(-0.533674141594226,-0.0742967091364493,
0.868149331745851));
#11272=CARTESIAN_POINT('Ctrl Pts',(-0.54708917182331,-0.115492077056649,
0.85981294420286));
#11273=CARTESIAN_POINT('Ctrl Pts',(-0.560922177770136,-0.141695629206859,
0.850993704737257));
#11274=CARTESIAN_POINT('Ctrl Pts',(-0.590422647829571,-0.181890537957859,
0.830754510485543));
#11275=CARTESIAN_POINT('Ctrl Pts',(-0.609616703125488,-0.201072148666545,
0.816896541396381));
#11276=CARTESIAN_POINT('Ctrl Pts',(-0.641117951819998,-0.223955109275652,
0.792310597819928));
#11277=CARTESIAN_POINT('Ctrl Pts',(-0.657208095763053,-0.232742381310829,
0.779109323683611));
#11278=CARTESIAN_POINT('Ctrl Pts',(-0.68964083160521,-0.244234834628584,
0.750552691816205));
#11279=CARTESIAN_POINT('Ctrl Pts',(-0.705971972091755,-0.246942143572133,
0.735185187071673));
#11280=CARTESIAN_POINT('Ctrl Pts',(-0.735185187071673,-0.246942143572133,
0.705971972091754));
#11281=CARTESIAN_POINT('Ctrl Pts',(-0.750552691816206,-0.244234834628584,
0.689640831605209));
#11282=CARTESIAN_POINT('Ctrl Pts',(-0.779109323683612,-0.232742381310829,
0.657208095763052));
#11283=CARTESIAN_POINT('Ctrl Pts',(-0.792310597819928,-0.223955109275652,
0.641117951819998));
#11284=CARTESIAN_POINT('Ctrl Pts',(-0.816896541396382,-0.201072148666545,
0.609616703125487));
#11285=CARTESIAN_POINT('Ctrl Pts',(-0.830754510485544,-0.181890537957858,
0.590422647829571));
#11286=CARTESIAN_POINT('Ctrl Pts',(-0.850993704737257,-0.141695629206858,
0.560922177770135));
#11287=CARTESIAN_POINT('Ctrl Pts',(-0.859812944202861,-0.115492077056649,
0.547089171823309));
#11288=CARTESIAN_POINT('Ctrl Pts',(-0.868149331745852,-0.0742967091364491,
0.533674141594226));
#11289=CARTESIAN_POINT('Ctrl Pts',(-0.870146645090731,-0.0609922781173483,
0.530395067942936));
#11290=CARTESIAN_POINT('Ctrl Pts',(-0.871530771444223,-0.04763,0.528110872004958));
#11291=CARTESIAN_POINT('',(-0.989696097314,-0.04763,0.242834539687906));
#11292=CARTESIAN_POINT('Origin',(0.,-0.04763,0.));
#11293=CARTESIAN_POINT('',(-1.019052,-0.246942143572133,1.248489836334E-16));
#11294=CARTESIAN_POINT('Ctrl Pts',(-0.989696097314,-0.04763,0.242834539687906));
#11295=CARTESIAN_POINT('Ctrl Pts',(-0.990332542620729,-0.0609922781173483,
0.24024064412003));
#11296=CARTESIAN_POINT('Ctrl Pts',(-0.991238884025248,-0.0742967091364492,
0.236509675094874));
#11297=CARTESIAN_POINT('Ctrl Pts',(-0.994830026707808,-0.115492077056649,
0.221129100087819));
#11298=CARTESIAN_POINT('Ctrl Pts',(-0.998375294985966,-0.141695629206859,
0.205111543747588));
#11299=CARTESIAN_POINT('Ctrl Pts',(-1.00492400591205,-0.181890537957859,
0.169940289819232));
#11300=CARTESIAN_POINT('Ctrl Pts',(-1.00869718865384,-0.201072148666545,
0.1465689792446));
#11301=CARTESIAN_POINT('Ctrl Pts',(-1.01358704779679,-0.223955109275652,
0.106909345252088));
#11302=CARTESIAN_POINT('Ctrl Pts',(-1.0156297872271,-0.232742381310829,
0.0861971848975944));
#11303=CARTESIAN_POINT('Ctrl Pts',(-1.01837060663223,-0.244234834628584,
0.0430711894098825));
#11304=CARTESIAN_POINT('Ctrl Pts',(-1.019052,-0.246942143572133,0.0206568624125608));
#11305=CARTESIAN_POINT('Ctrl Pts',(-1.019052,-0.246942143572133,1.2490009027033E-16));
#11306=CARTESIAN_POINT('',(-1.019052,-0.28578,1.24797876996471E-16));
#11307=CARTESIAN_POINT('',(-1.019052,-0.166705,1.24797876996471E-16));
#11308=CARTESIAN_POINT('Origin',(0.,-0.28578,0.));
#11309=CARTESIAN_POINT('',(-0.989696097314,-0.04763,-0.242834539687906));
#11310=CARTESIAN_POINT('Ctrl Pts',(-1.019052,-0.246942143572133,1.2490009027033E-16));
#11311=CARTESIAN_POINT('Ctrl Pts',(-1.019052,-0.246942143572133,-0.0206568624125605));
#11312=CARTESIAN_POINT('Ctrl Pts',(-1.01837060663223,-0.244234834628584,
-0.0430711894098822));
#11313=CARTESIAN_POINT('Ctrl Pts',(-1.0156297872271,-0.232742381310829,
-0.0861971848975941));
#11314=CARTESIAN_POINT('Ctrl Pts',(-1.01358704779679,-0.223955109275652,
-0.106909345252087));
#11315=CARTESIAN_POINT('Ctrl Pts',(-1.00869718865384,-0.201072148666546,
-0.1465689792446));
#11316=CARTESIAN_POINT('Ctrl Pts',(-1.00492400591205,-0.181890537957859,
-0.169940289819232));
#11317=CARTESIAN_POINT('Ctrl Pts',(-0.998375294985966,-0.141695629206859,
-0.205111543747588));
#11318=CARTESIAN_POINT('Ctrl Pts',(-0.994830026707808,-0.11549207705665,
-0.221129100087819));
#11319=CARTESIAN_POINT('Ctrl Pts',(-0.991238884025248,-0.0742967091364495,
-0.236509675094874));
#11320=CARTESIAN_POINT('Ctrl Pts',(-0.990332542620729,-0.0609922781173484,
-0.24024064412003));
#11321=CARTESIAN_POINT('Ctrl Pts',(-0.989696097314,-0.0476300000000001,
-0.242834539687907));
#11322=CARTESIAN_POINT('',(-0.871530771444223,-0.04763,-0.528110872004958));
#11323=CARTESIAN_POINT('Origin',(0.,-0.04763,0.));
#11324=CARTESIAN_POINT('',(-0.528110872004958,-0.04763,-0.871530771444223));
#11325=CARTESIAN_POINT('Ctrl Pts',(-0.871530771444223,-0.0476300000000001,
-0.528110872004958));
#11326=CARTESIAN_POINT('Ctrl Pts',(-0.87014664509073,-0.0609922781173484,
-0.530395067942936));
#11327=CARTESIAN_POINT('Ctrl Pts',(-0.868149331745851,-0.0742967091364494,
-0.533674141594226));
#11328=CARTESIAN_POINT('Ctrl Pts',(-0.85981294420286,-0.115492077056649,
-0.54708917182331));
#11329=CARTESIAN_POINT('Ctrl Pts',(-0.850993704737257,-0.141695629206859,
-0.560922177770136));
#11330=CARTESIAN_POINT('Ctrl Pts',(-0.830754510485543,-0.181890537957859,
-0.590422647829571));
#11331=CARTESIAN_POINT('Ctrl Pts',(-0.816896541396381,-0.201072148666546,
-0.609616703125488));
#11332=CARTESIAN_POINT('Ctrl Pts',(-0.792310597819928,-0.223955109275652,
-0.641117951819999));
#11333=CARTESIAN_POINT('Ctrl Pts',(-0.779109323683611,-0.232742381310829,
-0.657208095763053));
#11334=CARTESIAN_POINT('Ctrl Pts',(-0.750552691816205,-0.244234834628584,
-0.68964083160521));
#11335=CARTESIAN_POINT('Ctrl Pts',(-0.735185187071673,-0.246942143572133,
-0.705971972091755));
#11336=CARTESIAN_POINT('Ctrl Pts',(-0.705971972091754,-0.246942143572133,
-0.735185187071673));
#11337=CARTESIAN_POINT('Ctrl Pts',(-0.68964083160521,-0.244234834628584,
-0.750552691816206));
#11338=CARTESIAN_POINT('Ctrl Pts',(-0.657208095763052,-0.232742381310829,
-0.779109323683612));
#11339=CARTESIAN_POINT('Ctrl Pts',(-0.641117951819998,-0.223955109275652,
-0.792310597819928));
#11340=CARTESIAN_POINT('Ctrl Pts',(-0.609616703125488,-0.201072148666545,
-0.816896541396381));
#11341=CARTESIAN_POINT('Ctrl Pts',(-0.590422647829571,-0.181890537957859,
-0.830754510485543));
#11342=CARTESIAN_POINT('Ctrl Pts',(-0.560922177770136,-0.141695629206859,
-0.850993704737257));
#11343=CARTESIAN_POINT('Ctrl Pts',(-0.54708917182331,-0.115492077056649,
-0.85981294420286));
#11344=CARTESIAN_POINT('Ctrl Pts',(-0.533674141594226,-0.0742967091364494,
-0.868149331745852));
#11345=CARTESIAN_POINT('Ctrl Pts',(-0.530395067942936,-0.0609922781173484,
-0.870146645090731));
#11346=CARTESIAN_POINT('Ctrl Pts',(-0.528110872004958,-0.0476300000000001,
-0.871530771444223));
#11347=CARTESIAN_POINT('',(-0.242834539687906,-0.04763,-0.989696097314));
#11348=CARTESIAN_POINT('Origin',(0.,-0.04763,0.));
#11349=CARTESIAN_POINT('',(0.242834539687906,-0.04763,-0.989696097314));
#11350=CARTESIAN_POINT('Ctrl Pts',(-0.242834539687907,-0.04763,-0.989696097314));
#11351=CARTESIAN_POINT('Ctrl Pts',(-0.24024064412003,-0.0609922781173483,
-0.990332542620729));
#11352=CARTESIAN_POINT('Ctrl Pts',(-0.236509675094874,-0.0742967091364493,
-0.991238884025248));
#11353=CARTESIAN_POINT('Ctrl Pts',(-0.221129100087819,-0.115492077056649,
-0.994830026707808));
#11354=CARTESIAN_POINT('Ctrl Pts',(-0.205111543747588,-0.141695629206859,
-0.998375294985966));
#11355=CARTESIAN_POINT('Ctrl Pts',(-0.169940289819232,-0.181890537957859,
-1.00492400591205));
#11356=CARTESIAN_POINT('Ctrl Pts',(-0.1465689792446,-0.201072148666545,
-1.00869718865384));
#11357=CARTESIAN_POINT('Ctrl Pts',(-0.106909345252087,-0.223955109275652,
-1.01358704779679));
#11358=CARTESIAN_POINT('Ctrl Pts',(-0.0861971848975942,-0.232742381310829,
-1.0156297872271));
#11359=CARTESIAN_POINT('Ctrl Pts',(-0.0430711894098823,-0.244234834628584,
-1.01837060663223));
#11360=CARTESIAN_POINT('Ctrl Pts',(-0.0206568624125606,-0.246942143572133,
-1.019052));
#11361=CARTESIAN_POINT('Ctrl Pts',(0.0206568624125607,-0.246942143572133,
-1.019052));
#11362=CARTESIAN_POINT('Ctrl Pts',(0.0430711894098824,-0.244234834628584,
-1.01837060663223));
#11363=CARTESIAN_POINT('Ctrl Pts',(0.0861971848975943,-0.232742381310829,
-1.0156297872271));
#11364=CARTESIAN_POINT('Ctrl Pts',(0.106909345252088,-0.223955109275652,
-1.01358704779679));
#11365=CARTESIAN_POINT('Ctrl Pts',(0.1465689792446,-0.201072148666545,-1.00869718865384));
#11366=CARTESIAN_POINT('Ctrl Pts',(0.169940289819232,-0.181890537957859,
-1.00492400591205));
#11367=CARTESIAN_POINT('Ctrl Pts',(0.205111543747588,-0.141695629206859,
-0.998375294985966));
#11368=CARTESIAN_POINT('Ctrl Pts',(0.221129100087819,-0.115492077056649,
-0.994830026707808));
#11369=CARTESIAN_POINT('Ctrl Pts',(0.236509675094874,-0.0742967091364493,
-0.991238884025248));
#11370=CARTESIAN_POINT('Ctrl Pts',(0.24024064412003,-0.0609922781173484,
-0.990332542620729));
#11371=CARTESIAN_POINT('Ctrl Pts',(0.242834539687907,-0.04763,-0.989696097314));
#11372=CARTESIAN_POINT('',(0.528110872004958,-0.04763,-0.871530771444223));
#11373=CARTESIAN_POINT('Origin',(0.,-0.04763,0.));
#11374=CARTESIAN_POINT('',(0.871530771444223,-0.04763,-0.528110872004958));
#11375=CARTESIAN_POINT('Ctrl Pts',(0.528110872004958,-0.0476300000000001,
-0.871530771444223));
#11376=CARTESIAN_POINT('Ctrl Pts',(0.530395067942936,-0.0609922781173484,
-0.870146645090731));
#11377=CARTESIAN_POINT('Ctrl Pts',(0.533674141594226,-0.0742967091364493,
-0.868149331745851));
#11378=CARTESIAN_POINT('Ctrl Pts',(0.54708917182331,-0.115492077056649,
-0.85981294420286));
#11379=CARTESIAN_POINT('Ctrl Pts',(0.560922177770136,-0.141695629206859,
-0.850993704737257));
#11380=CARTESIAN_POINT('Ctrl Pts',(0.590422647829571,-0.181890537957859,
-0.830754510485543));
#11381=CARTESIAN_POINT('Ctrl Pts',(0.609616703125488,-0.201072148666545,
-0.816896541396381));
#11382=CARTESIAN_POINT('Ctrl Pts',(0.641117951819998,-0.223955109275652,
-0.792310597819928));
#11383=CARTESIAN_POINT('Ctrl Pts',(0.657208095763053,-0.232742381310829,
-0.779109323683612));
#11384=CARTESIAN_POINT('Ctrl Pts',(0.68964083160521,-0.244234834628584,
-0.750552691816206));
#11385=CARTESIAN_POINT('Ctrl Pts',(0.705971972091755,-0.246942143572133,
-0.735185187071673));
#11386=CARTESIAN_POINT('Ctrl Pts',(0.735185187071673,-0.246942143572133,
-0.705971972091754));
#11387=CARTESIAN_POINT('Ctrl Pts',(0.750552691816206,-0.244234834628584,
-0.68964083160521));
#11388=CARTESIAN_POINT('Ctrl Pts',(0.779109323683612,-0.232742381310829,
-0.657208095763053));
#11389=CARTESIAN_POINT('Ctrl Pts',(0.792310597819928,-0.223955109275652,
-0.641117951819998));
#11390=CARTESIAN_POINT('Ctrl Pts',(0.816896541396381,-0.201072148666545,
-0.609616703125488));
#11391=CARTESIAN_POINT('Ctrl Pts',(0.830754510485543,-0.181890537957859,
-0.590422647829571));
#11392=CARTESIAN_POINT('Ctrl Pts',(0.850993704737257,-0.141695629206859,
-0.560922177770136));
#11393=CARTESIAN_POINT('Ctrl Pts',(0.85981294420286,-0.115492077056649,
-0.54708917182331));
#11394=CARTESIAN_POINT('Ctrl Pts',(0.868149331745851,-0.0742967091364493,
-0.533674141594226));
#11395=CARTESIAN_POINT('Ctrl Pts',(0.870146645090731,-0.0609922781173484,
-0.530395067942936));
#11396=CARTESIAN_POINT('Ctrl Pts',(0.871530771444223,-0.0476300000000001,
-0.528110872004958));
#11397=CARTESIAN_POINT('',(0.989696097314,-0.04763,-0.242834539687906));
#11398=CARTESIAN_POINT('Origin',(0.,-0.04763,0.));
#11399=CARTESIAN_POINT('',(0.989696097314,-0.04763,0.242834539687906));
#11400=CARTESIAN_POINT('Ctrl Pts',(0.989696097314,-0.04763,-0.242834539687907));
#11401=CARTESIAN_POINT('Ctrl Pts',(0.990332542620729,-0.0609922781173483,
-0.24024064412003));
#11402=CARTESIAN_POINT('Ctrl Pts',(0.991238884025248,-0.0742967091364493,
-0.236509675094874));
#11403=CARTESIAN_POINT('Ctrl Pts',(0.994830026707808,-0.115492077056649,
-0.221129100087819));
#11404=CARTESIAN_POINT('Ctrl Pts',(0.998375294985966,-0.141695629206859,
-0.205111543747588));
#11405=CARTESIAN_POINT('Ctrl Pts',(1.00492400591205,-0.181890537957859,
-0.169940289819232));
#11406=CARTESIAN_POINT('Ctrl Pts',(1.00869718865384,-0.201072148666545,
-0.1465689792446));
#11407=CARTESIAN_POINT('Ctrl Pts',(1.01358704779679,-0.223955109275652,
-0.106909345252087));
#11408=CARTESIAN_POINT('Ctrl Pts',(1.0156297872271,-0.232742381310829,-0.0861971848975942));
#11409=CARTESIAN_POINT('Ctrl Pts',(1.01837060663223,-0.244234834628584,
-0.0430711894098823));
#11410=CARTESIAN_POINT('Ctrl Pts',(1.019052,-0.246942143572133,-0.0206568624125607));
#11411=CARTESIAN_POINT('Ctrl Pts',(1.019052,-0.246942143572133,0.0206568624125607));
#11412=CARTESIAN_POINT('Ctrl Pts',(1.01837060663223,-0.244234834628584,
0.0430711894098823));
#11413=CARTESIAN_POINT('Ctrl Pts',(1.0156297872271,-0.232742381310829,0.0861971848975942));
#11414=CARTESIAN_POINT('Ctrl Pts',(1.01358704779679,-0.223955109275652,
0.106909345252087));
#11415=CARTESIAN_POINT('Ctrl Pts',(1.00869718865384,-0.201072148666545,
0.1465689792446));
#11416=CARTESIAN_POINT('Ctrl Pts',(1.00492400591205,-0.181890537957859,
0.169940289819232));
#11417=CARTESIAN_POINT('Ctrl Pts',(0.998375294985966,-0.141695629206859,
0.205111543747588));
#11418=CARTESIAN_POINT('Ctrl Pts',(0.994830026707808,-0.115492077056649,
0.221129100087819));
#11419=CARTESIAN_POINT('Ctrl Pts',(0.991238884025248,-0.0742967091364492,
0.236509675094874));
#11420=CARTESIAN_POINT('Ctrl Pts',(0.990332542620729,-0.0609922781173483,
0.24024064412003));
#11421=CARTESIAN_POINT('Ctrl Pts',(0.989696097314,-0.04763,0.242834539687907));
#11422=CARTESIAN_POINT('Origin',(0.,-0.04763,0.));
#11423=CARTESIAN_POINT('Origin',(0.,-0.04763,0.));
#11424=CARTESIAN_POINT('',(0.238183666596899,-0.04763,0.951592097314));
#11425=CARTESIAN_POINT('Origin',(0.,-0.04763,0.));
#11426=CARTESIAN_POINT('Origin',(-1.94289029309402E-16,-0.04763,1.));
#11427=CARTESIAN_POINT('Origin',(-1.94289029309402E-16,0.,1.));
#11428=CARTESIAN_POINT('',(-0.2381836665969,-0.04763,0.951592097314));
#11429=CARTESIAN_POINT('Ctrl Pts',(-0.238183666596899,-0.0476299999999999,
0.951592097314));
#11430=CARTESIAN_POINT('Ctrl Pts',(-0.233157223576062,-0.0740444353928835,
0.952850216871763));
#11431=CARTESIAN_POINT('Ctrl Pts',(-0.223801617934946,-0.0999305678883309,
0.955173119738174));
#11432=CARTESIAN_POINT('Ctrl Pts',(-0.199966927975188,-0.142345102874864,
0.960411259488514));
#11433=CARTESIAN_POINT('Ctrl Pts',(-0.1868781821531,-0.159766064500479,
0.963103647174702));
#11434=CARTESIAN_POINT('Ctrl Pts',(-0.15681442133453,-0.190326085855194,
0.968453058988463));
#11435=CARTESIAN_POINT('Ctrl Pts',(-0.139836317888043,-0.203463743702801,
0.971100730005489));
#11436=CARTESIAN_POINT('Ctrl Pts',(-0.104422493053067,-0.224161999508995,
0.975530745318961));
#11437=CARTESIAN_POINT('Ctrl Pts',(-0.0842175114474176,-0.232861760990032,
0.977553872336861));
#11438=CARTESIAN_POINT('Ctrl Pts',(-0.0421062857595701,-0.244251601209411,
0.980270995488453));
#11439=CARTESIAN_POINT('Ctrl Pts',(-0.0201990724523197,-0.246942143572133,
0.980948));
#11440=CARTESIAN_POINT('Ctrl Pts',(0.020199072452319,-0.246942143572133,
0.980948));
#11441=CARTESIAN_POINT('Ctrl Pts',(0.0421062857595694,-0.244251601209411,
0.980270995488454));
#11442=CARTESIAN_POINT('Ctrl Pts',(0.0842175114474169,-0.232861760990032,
0.977553872336861));
#11443=CARTESIAN_POINT('Ctrl Pts',(0.104422493053067,-0.224161999508995,
0.975530745318961));
#11444=CARTESIAN_POINT('Ctrl Pts',(0.139836317888042,-0.203463743702801,
0.971100730005489));
#11445=CARTESIAN_POINT('Ctrl Pts',(0.15681442133453,-0.190326085855194,
0.968453058988463));
#11446=CARTESIAN_POINT('Ctrl Pts',(0.1868781821531,-0.15976606450048,0.963103647174702));
#11447=CARTESIAN_POINT('Ctrl Pts',(0.199966927975188,-0.142345102874864,
0.960411259488514));
#11448=CARTESIAN_POINT('Ctrl Pts',(0.223801617934945,-0.0999305678883309,
0.955173119738174));
#11449=CARTESIAN_POINT('Ctrl Pts',(0.233157223576061,-0.0740444353928835,
0.952850216871763));
#11450=CARTESIAN_POINT('Ctrl Pts',(0.238183666596899,-0.0476299999999999,
0.951592097314));
#11451=CARTESIAN_POINT('Origin',(-1.94289029309402E-16,-0.04763,1.));
#11452=CARTESIAN_POINT('Origin',(0.,-0.04763,0.));
#11453=CARTESIAN_POINT('',(-0.504455939115715,-0.04763,0.841298510752802));
#11454=CARTESIAN_POINT('Origin',(0.,-0.04763,0.));
#11455=CARTESIAN_POINT('Origin',(-0.707106781186548,-0.04763,0.707106781186547));
#11456=CARTESIAN_POINT('Origin',(-0.707106781186548,0.,0.707106781186547));
#11457=CARTESIAN_POINT('',(-0.841298510752802,-0.04763,0.504455939115715));
#11458=CARTESIAN_POINT('Ctrl Pts',(-0.841298510752802,-0.04763,0.504455939115715));
#11459=CARTESIAN_POINT('Ctrl Pts',(-0.838633903678357,-0.0740444353928835,
0.508899795931835));
#11460=CARTESIAN_POINT('Ctrl Pts',(-0.833661031856294,-0.0999305678883309,
0.517157748491652));
#11461=CARTESIAN_POINT('Ctrl Pts',(-0.820511285096538,-0.142345102874864,
0.537715343527944));
#11462=CARTESIAN_POINT('Ctrl Pts',(-0.813159949759,-0.159766064500479,0.548874290046456));
#11463=CARTESIAN_POINT('Ctrl Pts',(-0.795684265985089,-0.190326085855194,
0.573915184558107));
#11464=CARTESIAN_POINT('Ctrl Pts',(-0.78555112003688,-0.203463743702801,
0.587792702767295));
#11465=CARTESIAN_POINT('Ctrl Pts',(-0.763642258217233,-0.224161999508995,
0.615966552324775));
#11466=CARTESIAN_POINT('Ctrl Pts',(-0.750785745543687,-0.232861760990032,
0.631684198665438));
#11467=CARTESIAN_POINT('Ctrl Pts',(-0.722929908501543,-0.244251601209411,
0.663382628119203));
#11468=CARTESIAN_POINT('Ctrl Pts',(-0.707917883896095,-0.246942143572133,
0.679352081686668));
#11469=CARTESIAN_POINT('Ctrl Pts',(-0.679352081686668,-0.246942143572133,
0.707917883896095));
#11470=CARTESIAN_POINT('Ctrl Pts',(-0.663382628119203,-0.244251601209411,
0.722929908501544));
#11471=CARTESIAN_POINT('Ctrl Pts',(-0.631684198665438,-0.232861760990031,
0.750785745543687));
#11472=CARTESIAN_POINT('Ctrl Pts',(-0.615966552324775,-0.224161999508995,
0.763642258217233));
#11473=CARTESIAN_POINT('Ctrl Pts',(-0.587792702767295,-0.203463743702801,
0.78555112003688));
#11474=CARTESIAN_POINT('Ctrl Pts',(-0.573915184558107,-0.190326085855194,
0.795684265985088));
#11475=CARTESIAN_POINT('Ctrl Pts',(-0.548874290046456,-0.159766064500479,
0.813159949759));
#11476=CARTESIAN_POINT('Ctrl Pts',(-0.537715343527944,-0.142345102874864,
0.820511285096538));
#11477=CARTESIAN_POINT('Ctrl Pts',(-0.517157748491652,-0.0999305678883309,
0.833661031856294));
#11478=CARTESIAN_POINT('Ctrl Pts',(-0.508899795931835,-0.0740444353928835,
0.838633903678357));
#11479=CARTESIAN_POINT('Ctrl Pts',(-0.504455939115716,-0.04763,0.841298510752801));
#11480=CARTESIAN_POINT('Origin',(-0.707106781186548,-0.04763,0.707106781186547));
#11481=CARTESIAN_POINT('Origin',(0.,-0.04763,0.));
#11482=CARTESIAN_POINT('',(-0.951592097314,-0.04763,0.238183666596899));
#11483=CARTESIAN_POINT('Origin',(0.,-0.04763,0.));
#11484=CARTESIAN_POINT('Origin',(-1.,-0.04763,-1.11022302462516E-16));
#11485=CARTESIAN_POINT('Origin',(-1.,0.,-1.11022302462516E-16));
#11486=CARTESIAN_POINT('',(-0.951592097314,-0.04763,-0.2381836665969));
#11487=CARTESIAN_POINT('',(-0.980948,-0.246942143572133,1.08514323328844E-18));
#11488=CARTESIAN_POINT('Ctrl Pts',(-0.951592097314,-0.04763,-0.238183666596899));
#11489=CARTESIAN_POINT('Ctrl Pts',(-0.952850216871763,-0.0740444353928835,
-0.233157223576062));
#11490=CARTESIAN_POINT('Ctrl Pts',(-0.955173119738174,-0.0999305678883309,
-0.223801617934946));
#11491=CARTESIAN_POINT('Ctrl Pts',(-0.960411259488514,-0.142345102874864,
-0.199966927975188));
#11492=CARTESIAN_POINT('Ctrl Pts',(-0.963103647174702,-0.159766064500479,
-0.1868781821531));
#11493=CARTESIAN_POINT('Ctrl Pts',(-0.968453058988463,-0.190326085855194,
-0.15681442133453));
#11494=CARTESIAN_POINT('Ctrl Pts',(-0.971100730005489,-0.203463743702801,
-0.139836317888043));
#11495=CARTESIAN_POINT('Ctrl Pts',(-0.975530745318961,-0.224161999508995,
-0.104422493053067));
#11496=CARTESIAN_POINT('Ctrl Pts',(-0.977553872336861,-0.232861760990032,
-0.0842175114474175));
#11497=CARTESIAN_POINT('Ctrl Pts',(-0.980270995488453,-0.244251601209411,
-0.0421062857595699));
#11498=CARTESIAN_POINT('Ctrl Pts',(-0.980948,-0.246942143572133,-0.0201990724523195));
#11499=CARTESIAN_POINT('Ctrl Pts',(-0.980948,-0.246942143572133,-1.17961196366423E-16));
#11500=CARTESIAN_POINT('Origin',(-1.,-0.04763,-1.11022302462516E-16));
#11501=CARTESIAN_POINT('Ctrl Pts',(-0.980948,-0.246942143572133,-1.17961196366423E-16));
#11502=CARTESIAN_POINT('Ctrl Pts',(-0.980948,-0.246942143572133,0.0201990724523192));
#11503=CARTESIAN_POINT('Ctrl Pts',(-0.980270995488453,-0.244251601209411,
0.0421062857595695));
#11504=CARTESIAN_POINT('Ctrl Pts',(-0.977553872336861,-0.232861760990032,
0.0842175114474169));
#11505=CARTESIAN_POINT('Ctrl Pts',(-0.975530745318961,-0.224161999508995,
0.104422493053066));
#11506=CARTESIAN_POINT('Ctrl Pts',(-0.971100730005489,-0.203463743702801,
0.139836317888042));
#11507=CARTESIAN_POINT('Ctrl Pts',(-0.968453058988463,-0.190326085855194,
0.15681442133453));
#11508=CARTESIAN_POINT('Ctrl Pts',(-0.963103647174702,-0.15976606450048,
0.1868781821531));
#11509=CARTESIAN_POINT('Ctrl Pts',(-0.960411259488514,-0.142345102874864,
0.199966927975188));
#11510=CARTESIAN_POINT('Ctrl Pts',(-0.955173119738174,-0.099930567888331,
0.223801617934945));
#11511=CARTESIAN_POINT('Ctrl Pts',(-0.952850216871763,-0.0740444353928835,
0.233157223576061));
#11512=CARTESIAN_POINT('Ctrl Pts',(-0.951592097314,-0.04763,0.238183666596899));
#11513=CARTESIAN_POINT('Origin',(0.,-0.04763,0.));
#11514=CARTESIAN_POINT('',(-0.841298510752802,-0.04763,-0.504455939115715));
#11515=CARTESIAN_POINT('Origin',(0.,-0.04763,0.));
#11516=CARTESIAN_POINT('Origin',(-0.707106781186547,-0.04763,-0.707106781186548));
#11517=CARTESIAN_POINT('Origin',(-0.707106781186547,0.,-0.707106781186548));
#11518=CARTESIAN_POINT('',(-0.504455939115715,-0.04763,-0.841298510752802));
#11519=CARTESIAN_POINT('Ctrl Pts',(-0.504455939115715,-0.04763,-0.841298510752802));
#11520=CARTESIAN_POINT('Ctrl Pts',(-0.508899795931835,-0.0740444353928835,
-0.838633903678357));
#11521=CARTESIAN_POINT('Ctrl Pts',(-0.517157748491652,-0.0999305678883309,
-0.833661031856294));
#11522=CARTESIAN_POINT('Ctrl Pts',(-0.537715343527944,-0.142345102874864,
-0.820511285096538));
#11523=CARTESIAN_POINT('Ctrl Pts',(-0.548874290046456,-0.159766064500479,
-0.813159949759));
#11524=CARTESIAN_POINT('Ctrl Pts',(-0.573915184558107,-0.190326085855194,
-0.795684265985089));
#11525=CARTESIAN_POINT('Ctrl Pts',(-0.587792702767295,-0.203463743702801,
-0.78555112003688));
#11526=CARTESIAN_POINT('Ctrl Pts',(-0.615966552324775,-0.224161999508995,
-0.763642258217233));
#11527=CARTESIAN_POINT('Ctrl Pts',(-0.631684198665438,-0.232861760990032,
-0.750785745543687));
#11528=CARTESIAN_POINT('Ctrl Pts',(-0.663382628119203,-0.244251601209411,
-0.722929908501543));
#11529=CARTESIAN_POINT('Ctrl Pts',(-0.679352081686668,-0.246942143572133,
-0.707917883896095));
#11530=CARTESIAN_POINT('Ctrl Pts',(-0.707917883896095,-0.246942143572133,
-0.679352081686668));
#11531=CARTESIAN_POINT('Ctrl Pts',(-0.722929908501543,-0.244251601209411,
-0.663382628119203));
#11532=CARTESIAN_POINT('Ctrl Pts',(-0.750785745543687,-0.232861760990032,
-0.631684198665439));
#11533=CARTESIAN_POINT('Ctrl Pts',(-0.763642258217232,-0.224161999508995,
-0.615966552324775));
#11534=CARTESIAN_POINT('Ctrl Pts',(-0.78555112003688,-0.203463743702801,
-0.587792702767295));
#11535=CARTESIAN_POINT('Ctrl Pts',(-0.795684265985088,-0.190326085855194,
-0.573915184558107));
#11536=CARTESIAN_POINT('Ctrl Pts',(-0.813159949759,-0.15976606450048,-0.548874290046456));
#11537=CARTESIAN_POINT('Ctrl Pts',(-0.820511285096538,-0.142345102874864,
-0.537715343527944));
#11538=CARTESIAN_POINT('Ctrl Pts',(-0.833661031856294,-0.0999305678883311,
-0.517157748491652));
#11539=CARTESIAN_POINT('Ctrl Pts',(-0.838633903678357,-0.0740444353928836,
-0.508899795931835));
#11540=CARTESIAN_POINT('Ctrl Pts',(-0.841298510752801,-0.04763,-0.504455939115715));
#11541=CARTESIAN_POINT('Origin',(-0.707106781186547,-0.04763,-0.707106781186548));
#11542=CARTESIAN_POINT('Origin',(0.,-0.04763,0.));
#11543=CARTESIAN_POINT('',(-0.238183666596899,-0.04763,-0.951592097314));
#11544=CARTESIAN_POINT('Origin',(0.,-0.04763,0.));
#11545=CARTESIAN_POINT('Origin',(5.55111512312578E-17,-0.04763,-1.));
#11546=CARTESIAN_POINT('Origin',(5.55111512312578E-17,0.,-1.));
#11547=CARTESIAN_POINT('',(0.238183666596899,-0.04763,-0.951592097314));
#11548=CARTESIAN_POINT('Ctrl Pts',(0.238183666596899,-0.04763,-0.951592097314));
#11549=CARTESIAN_POINT('Ctrl Pts',(0.233157223576062,-0.0740444353928835,
-0.952850216871763));
#11550=CARTESIAN_POINT('Ctrl Pts',(0.223801617934946,-0.099930567888331,
-0.955173119738174));
#11551=CARTESIAN_POINT('Ctrl Pts',(0.199966927975188,-0.142345102874864,
-0.960411259488514));
#11552=CARTESIAN_POINT('Ctrl Pts',(0.1868781821531,-0.15976606450048,-0.963103647174702));
#11553=CARTESIAN_POINT('Ctrl Pts',(0.15681442133453,-0.190326085855194,
-0.968453058988463));
#11554=CARTESIAN_POINT('Ctrl Pts',(0.139836317888042,-0.203463743702801,
-0.971100730005489));
#11555=CARTESIAN_POINT('Ctrl Pts',(0.104422493053067,-0.224161999508995,
-0.975530745318961));
#11556=CARTESIAN_POINT('Ctrl Pts',(0.0842175114474173,-0.232861760990032,
-0.977553872336861));
#11557=CARTESIAN_POINT('Ctrl Pts',(0.0421062857595698,-0.244251601209411,
-0.980270995488453));
#11558=CARTESIAN_POINT('Ctrl Pts',(0.0201990724523194,-0.246942143572133,
-0.980948));
#11559=CARTESIAN_POINT('Ctrl Pts',(-0.0201990724523193,-0.246942143572133,
-0.980948));
#11560=CARTESIAN_POINT('Ctrl Pts',(-0.0421062857595697,-0.244251601209411,
-0.980270995488453));
#11561=CARTESIAN_POINT('Ctrl Pts',(-0.0842175114474171,-0.232861760990032,
-0.977553872336861));
#11562=CARTESIAN_POINT('Ctrl Pts',(-0.104422493053067,-0.224161999508995,
-0.975530745318961));
#11563=CARTESIAN_POINT('Ctrl Pts',(-0.139836317888042,-0.203463743702801,
-0.971100730005489));
#11564=CARTESIAN_POINT('Ctrl Pts',(-0.15681442133453,-0.190326085855194,
-0.968453058988463));
#11565=CARTESIAN_POINT('Ctrl Pts',(-0.1868781821531,-0.15976606450048,-0.963103647174702));
#11566=CARTESIAN_POINT('Ctrl Pts',(-0.199966927975188,-0.142345102874864,
-0.960411259488514));
#11567=CARTESIAN_POINT('Ctrl Pts',(-0.223801617934945,-0.099930567888331,
-0.955173119738174));
#11568=CARTESIAN_POINT('Ctrl Pts',(-0.233157223576062,-0.0740444353928835,
-0.952850216871763));
#11569=CARTESIAN_POINT('Ctrl Pts',(-0.238183666596899,-0.0476299999999999,
-0.951592097314));
#11570=CARTESIAN_POINT('Origin',(5.55111512312578E-17,-0.04763,-1.));
#11571=CARTESIAN_POINT('Origin',(0.,-0.04763,0.));
#11572=CARTESIAN_POINT('',(0.504455939115715,-0.04763,-0.841298510752802));
#11573=CARTESIAN_POINT('Origin',(0.,-0.04763,0.));
#11574=CARTESIAN_POINT('Origin',(0.707106781186548,-0.04763,-0.707106781186547));
#11575=CARTESIAN_POINT('Origin',(0.707106781186548,0.,-0.707106781186547));
#11576=CARTESIAN_POINT('',(0.841298510752802,-0.04763,-0.504455939115715));
#11577=CARTESIAN_POINT('Ctrl Pts',(0.841298510752802,-0.04763,-0.504455939115715));
#11578=CARTESIAN_POINT('Ctrl Pts',(0.838633903678357,-0.0740444353928835,
-0.508899795931835));
#11579=CARTESIAN_POINT('Ctrl Pts',(0.833661031856294,-0.0999305678883309,
-0.517157748491652));
#11580=CARTESIAN_POINT('Ctrl Pts',(0.820511285096538,-0.142345102874864,
-0.537715343527944));
#11581=CARTESIAN_POINT('Ctrl Pts',(0.813159949759,-0.159766064500479,-0.548874290046456));
#11582=CARTESIAN_POINT('Ctrl Pts',(0.795684265985088,-0.190326085855194,
-0.573915184558107));
#11583=CARTESIAN_POINT('Ctrl Pts',(0.78555112003688,-0.203463743702801,
-0.587792702767295));
#11584=CARTESIAN_POINT('Ctrl Pts',(0.763642258217233,-0.224161999508995,
-0.615966552324775));
#11585=CARTESIAN_POINT('Ctrl Pts',(0.750785745543687,-0.232861760990032,
-0.631684198665438));
#11586=CARTESIAN_POINT('Ctrl Pts',(0.722929908501543,-0.244251601209411,
-0.663382628119203));
#11587=CARTESIAN_POINT('Ctrl Pts',(0.707917883896095,-0.246942143572133,
-0.679352081686668));
#11588=CARTESIAN_POINT('Ctrl Pts',(0.679352081686668,-0.246942143572133,
-0.707917883896095));
#11589=CARTESIAN_POINT('Ctrl Pts',(0.663382628119203,-0.244251601209411,
-0.722929908501543));
#11590=CARTESIAN_POINT('Ctrl Pts',(0.631684198665438,-0.232861760990032,
-0.750785745543687));
#11591=CARTESIAN_POINT('Ctrl Pts',(0.615966552324775,-0.224161999508995,
-0.763642258217232));
#11592=CARTESIAN_POINT('Ctrl Pts',(0.587792702767295,-0.203463743702801,
-0.78555112003688));
#11593=CARTESIAN_POINT('Ctrl Pts',(0.573915184558107,-0.190326085855194,
-0.795684265985088));
#11594=CARTESIAN_POINT('Ctrl Pts',(0.548874290046456,-0.159766064500479,
-0.813159949759));
#11595=CARTESIAN_POINT('Ctrl Pts',(0.537715343527944,-0.142345102874864,
-0.820511285096538));
#11596=CARTESIAN_POINT('Ctrl Pts',(0.517157748491652,-0.099930567888331,
-0.833661031856294));
#11597=CARTESIAN_POINT('Ctrl Pts',(0.508899795931835,-0.0740444353928835,
-0.838633903678357));
#11598=CARTESIAN_POINT('Ctrl Pts',(0.504455939115715,-0.04763,-0.841298510752801));
#11599=CARTESIAN_POINT('Origin',(0.707106781186548,-0.04763,-0.707106781186547));
#11600=CARTESIAN_POINT('Origin',(0.,-0.166705,0.));
#11601=CARTESIAN_POINT('',(-0.980948,-0.28578,1.20131482833E-16));
#11602=CARTESIAN_POINT('Origin',(0.,-0.28578,0.));
#11603=CARTESIAN_POINT('',(-0.980948,-0.166705,1.20131482833E-16));
#11604=CARTESIAN_POINT('',(0.951592097314,-0.04763,0.238183666596899));
#11605=CARTESIAN_POINT('Origin',(0.,-0.04763,0.));
#11606=CARTESIAN_POINT('',(0.951592097314,-0.04763,-0.238183666596899));
#11607=CARTESIAN_POINT('Ctrl Pts',(0.951592097314,-0.04763,0.238183666596899));
#11608=CARTESIAN_POINT('Ctrl Pts',(0.952850216871763,-0.0740444353928835,
0.233157223576062));
#11609=CARTESIAN_POINT('Ctrl Pts',(0.955173119738174,-0.099930567888331,
0.223801617934945));
#11610=CARTESIAN_POINT('Ctrl Pts',(0.960411259488514,-0.142345102874864,
0.199966927975188));
#11611=CARTESIAN_POINT('Ctrl Pts',(0.963103647174702,-0.15976606450048,
0.1868781821531));
#11612=CARTESIAN_POINT('Ctrl Pts',(0.968453058988463,-0.190326085855194,
0.15681442133453));
#11613=CARTESIAN_POINT('Ctrl Pts',(0.971100730005489,-0.203463743702801,
0.139836317888042));
#11614=CARTESIAN_POINT('Ctrl Pts',(0.975530745318961,-0.224161999508995,
0.104422493053067));
#11615=CARTESIAN_POINT('Ctrl Pts',(0.977553872336861,-0.232861760990032,
0.0842175114474172));
#11616=CARTESIAN_POINT('Ctrl Pts',(0.980270995488453,-0.244251601209411,
0.0421062857595697));
#11617=CARTESIAN_POINT('Ctrl Pts',(0.980948,-0.246942143572133,0.0201990724523194));
#11618=CARTESIAN_POINT('Ctrl Pts',(0.980948,-0.246942143572133,-0.0201990724523194));
#11619=CARTESIAN_POINT('Ctrl Pts',(0.980270995488453,-0.244251601209411,
-0.0421062857595697));
#11620=CARTESIAN_POINT('Ctrl Pts',(0.977553872336861,-0.232861760990032,
-0.0842175114474172));
#11621=CARTESIAN_POINT('Ctrl Pts',(0.975530745318961,-0.224161999508995,
-0.104422493053067));
#11622=CARTESIAN_POINT('Ctrl Pts',(0.971100730005489,-0.203463743702801,
-0.139836317888042));
#11623=CARTESIAN_POINT('Ctrl Pts',(0.968453058988463,-0.190326085855194,
-0.15681442133453));
#11624=CARTESIAN_POINT('Ctrl Pts',(0.963103647174702,-0.15976606450048,
-0.1868781821531));
#11625=CARTESIAN_POINT('Ctrl Pts',(0.960411259488514,-0.142345102874864,
-0.199966927975188));
#11626=CARTESIAN_POINT('Ctrl Pts',(0.955173119738174,-0.099930567888331,
-0.223801617934945));
#11627=CARTESIAN_POINT('Ctrl Pts',(0.952850216871763,-0.0740444353928835,
-0.233157223576062));
#11628=CARTESIAN_POINT('Ctrl Pts',(0.951592097314,-0.0476299999999999,-0.238183666596899));
#11629=CARTESIAN_POINT('Origin',(0.,-0.04763,0.));
#11630=CARTESIAN_POINT('Origin',(0.,-0.04763,0.));
#11631=CARTESIAN_POINT('Origin',(1.,-0.04763,0.));
#11632=CARTESIAN_POINT('Origin',(1.,0.,0.));
#11633=CARTESIAN_POINT('Origin',(1.,-0.04763,0.));
#11634=CARTESIAN_POINT('Origin',(0.,-0.28578,0.));
#11635=CARTESIAN_POINT('Origin',(0.,-0.04763,0.));
#11636=CARTESIAN_POINT('',(0.,0.,0.));
#11637=CARTESIAN_POINT('Origin',(1.013815,0.445,0.));
#11638=CARTESIAN_POINT('',(-1.013815,0.445,-1.24156529467757E-16));
#11639=CARTESIAN_POINT('Origin',(0.,0.445,0.));
#11640=CARTESIAN_POINT('',(-0.991185,0.445,-1.21385153761287E-16));
#11641=CARTESIAN_POINT('Origin',(0.,0.445,0.));
#11642=CARTESIAN_POINT('Origin',(0.,0.4075,0.));
#11643=CARTESIAN_POINT('',(-1.013815,0.37,-1.24156529467757E-16));
#11644=CARTESIAN_POINT('Origin',(0.,0.37,0.));
#11645=CARTESIAN_POINT('',(-1.013815,0.4075,-1.24156529467757E-16));
#11646=CARTESIAN_POINT('Origin',(0.991185,0.37,0.));
#11647=CARTESIAN_POINT('',(-0.991185,0.37,-1.21385153761287E-16));
#11648=CARTESIAN_POINT('Origin',(0.,0.37,0.));
#11649=CARTESIAN_POINT('Origin',(0.,0.4075,0.));
#11650=CARTESIAN_POINT('',(-0.991185,0.4075,-1.21385153761287E-16));
#11651=CARTESIAN_POINT('Origin',(1.013815,-0.37,0.));
#11652=CARTESIAN_POINT('',(-1.013815,-0.37,-1.24156529467757E-16));
#11653=CARTESIAN_POINT('Origin',(0.,-0.37,0.));
#11654=CARTESIAN_POINT('',(-0.991185,-0.37,-1.21385153761287E-16));
#11655=CARTESIAN_POINT('Origin',(0.,-0.37,0.));
#11656=CARTESIAN_POINT('Origin',(0.,-0.4075,0.));
#11657=CARTESIAN_POINT('',(-1.013815,-0.445,-1.24156529467757E-16));
#11658=CARTESIAN_POINT('Origin',(0.,-0.445,0.));
#11659=CARTESIAN_POINT('',(-1.013815,-0.4075,-1.24156529467757E-16));
#11660=CARTESIAN_POINT('Origin',(0.991185,-0.445,0.));
#11661=CARTESIAN_POINT('',(-0.991185,-0.445,-1.21385153761287E-16));
#11662=CARTESIAN_POINT('Origin',(0.,-0.445,0.));
#11663=CARTESIAN_POINT('Origin',(0.,-0.4075,0.));
#11664=CARTESIAN_POINT('',(-0.991185,-0.4075,-1.21385153761287E-16));
#11665=CARTESIAN_POINT('',(0.,0.,0.));
#11666=CARTESIAN_POINT('',(0.,0.,0.));
#11667=CARTESIAN_POINT('',(0.,0.,0.));
#11668=CARTESIAN_POINT('',(0.,0.,0.));
#11669=CARTESIAN_POINT('',(0.,0.,0.));
#11670=CARTESIAN_POINT('',(0.,0.,0.));
#11671=CARTESIAN_POINT('Origin',(0.,-0.7,0.));
#11672=CARTESIAN_POINT('',(-0.1954,-0.7,2.39295984553393E-17));
#11673=CARTESIAN_POINT('Origin',(0.,-0.7,0.));
#11674=CARTESIAN_POINT('Origin',(0.3,0.4,0.));
#11675=CARTESIAN_POINT('',(-0.3,0.4,-3.67394039744206E-17));
#11676=CARTESIAN_POINT('Origin',(0.,0.4,0.));
#11677=CARTESIAN_POINT('Origin',(0.,0.375,0.));
#11678=CARTESIAN_POINT('',(-0.35,0.35,-4.28626379701573E-17));
#11679=CARTESIAN_POINT('Origin',(0.,0.35,0.));
#11680=CARTESIAN_POINT('',(-0.325,0.375,-3.9801020972289E-17));
#11681=CARTESIAN_POINT('Origin',(0.,0.19,0.));
#11682=CARTESIAN_POINT('',(-0.35,0.03,-4.28626379701574E-17));
#11683=CARTESIAN_POINT('Origin',(0.,0.03,0.));
#11684=CARTESIAN_POINT('',(-0.35,0.19,-4.28626379701574E-17));
#11685=CARTESIAN_POINT('Origin',(0.,0.0149999999999999,0.));
#11686=CARTESIAN_POINT('',(-0.32,-3.29597460435593E-17,-3.91886975727153E-17));
#11687=CARTESIAN_POINT('Origin',(0.,0.,0.));
#11688=CARTESIAN_POINT('',(-0.335,0.0149999999999999,-4.10256677714363E-17));
#11689=CARTESIAN_POINT('Origin',(0.22,0.,0.));
#11690=CARTESIAN_POINT('',(-0.22,-6.93889390390723E-18,-2.69422295812418E-17));
#11691=CARTESIAN_POINT('Origin',(0.,0.,0.));
#11692=CARTESIAN_POINT('Origin',(0.,-0.02,0.));
#11693=CARTESIAN_POINT('',(-0.1954,-0.0492,2.39295984553393E-17));
#11694=CARTESIAN_POINT('Origin',(0.,-0.0492,0.));
#11695=CARTESIAN_POINT('',(-0.21,-0.02,-2.57175827820944E-17));
#11696=CARTESIAN_POINT('Origin',(0.,-0.8,0.));
#11697=CARTESIAN_POINT('',(-0.1954,-0.8,-2.39295984553393E-17));
#11698=CARTESIAN_POINT('Origin',(0.0866025403784439,-0.4,-0.15));
#11699=CARTESIAN_POINT('',(0.173205080756888,-0.4,0.));
#11700=CARTESIAN_POINT('',(0.0866025403784439,-0.4,-0.15));
#11701=CARTESIAN_POINT('',(0.173205080756888,-0.4,0.));
#11702=CARTESIAN_POINT('',(0.0866025403784439,-0.64,-0.15));
#11703=CARTESIAN_POINT('',(0.0866025403784439,-0.4,-0.15));
#11704=CARTESIAN_POINT('',(0.173205080756888,-0.64,0.));
#11705=CARTESIAN_POINT('',(0.173205080756888,-0.64,0.));
#11706=CARTESIAN_POINT('',(0.173205080756888,-0.4,0.));
#11707=CARTESIAN_POINT('Origin',(-0.0866025403784438,-0.4,-0.15));
#11708=CARTESIAN_POINT('',(-0.0866025403784438,-0.4,-0.15));
#11709=CARTESIAN_POINT('',(0.0866025403784439,-0.4,-0.15));
#11710=CARTESIAN_POINT('',(-0.0866025403784438,-0.64,-0.15));
#11711=CARTESIAN_POINT('',(-0.0866025403784438,-0.4,-0.15));
#11712=CARTESIAN_POINT('',(0.0866025403784439,-0.64,-0.15));
#11713=CARTESIAN_POINT('Origin',(-0.173205080756888,-0.4,-2.77555756156289E-17));
#11714=CARTESIAN_POINT('',(-0.173205080756888,-0.4,-2.12115047744981E-17));
#11715=CARTESIAN_POINT('',(-0.0866025403784438,-0.4,-0.15));
#11716=CARTESIAN_POINT('',(-0.173205080756888,-0.64,-2.77555756156289E-17));
#11717=CARTESIAN_POINT('',(-0.173205080756888,-0.4,-2.12115047744981E-17));
#11718=CARTESIAN_POINT('',(-0.0866025403784438,-0.64,-0.15));
#11719=CARTESIAN_POINT('Origin',(-0.0866025403784439,-0.4,0.15));
#11720=CARTESIAN_POINT('',(-0.0866025403784439,-0.4,0.15));
#11721=CARTESIAN_POINT('',(-0.173205080756888,-0.4,-2.12115047744981E-17));
#11722=CARTESIAN_POINT('',(-0.0866025403784439,-0.64,0.15));
#11723=CARTESIAN_POINT('',(-0.0866025403784439,-0.4,0.15));
#11724=CARTESIAN_POINT('',(-0.173205080756888,-0.64,-2.12115047744981E-17));
#11725=CARTESIAN_POINT('Origin',(0.0866025403784439,-0.4,0.15));
#11726=CARTESIAN_POINT('',(0.0866025403784439,-0.4,0.15));
#11727=CARTESIAN_POINT('',(-0.0866025403784439,-0.4,0.15));
#11728=CARTESIAN_POINT('',(0.0866025403784439,-0.64,0.15));
#11729=CARTESIAN_POINT('',(0.0866025403784439,-0.4,0.15));
#11730=CARTESIAN_POINT('',(-0.0866025403784439,-0.64,0.15));
#11731=CARTESIAN_POINT('Origin',(0.173205080756888,-0.4,0.));
#11732=CARTESIAN_POINT('',(0.0866025403784439,-0.4,0.15));
#11733=CARTESIAN_POINT('',(0.0866025403784439,-0.64,0.15));
#11734=CARTESIAN_POINT('Origin',(0.,-0.4,-2.77555756156289E-17));
#11735=CARTESIAN_POINT('Origin',(0.,-0.64,-2.77555756156289E-17));
#11736=CARTESIAN_POINT('',(0.,0.,0.));
#11737=CARTESIAN_POINT('',(0.,0.,0.));
#11738=CARTESIAN_POINT('',(0.,0.,0.));
#11739=CARTESIAN_POINT('',(0.,0.,0.));
#11740=CARTESIAN_POINT('',(0.,0.,0.));
#11741=CARTESIAN_POINT('',(0.,0.,0.));
#11742=CARTESIAN_POINT('',(0.,0.,5.5));
#11743=CARTESIAN_POINT('',(1.23743686707646,1.23743686707646,4.7));
#11744=CARTESIAN_POINT('',(-1.23743686707646,1.23743686707646,4.7));
#11745=CARTESIAN_POINT('',(-1.23743686707646,-1.23743686707646,4.7));
#11746=CARTESIAN_POINT('',(1.23743686707646,-1.23743686707646,4.7));
#11747=CARTESIAN_POINT('',(1.23743686707646,1.23743686707646,6.3));
#11748=CARTESIAN_POINT('',(-1.23743686707646,1.23743686707646,6.3));
#11749=CARTESIAN_POINT('',(-1.23743686707646,-1.23743686707646,6.3));
#11750=CARTESIAN_POINT('',(1.23743686707646,-1.23743686707646,6.3));
#11751=CARTESIAN_POINT('',(9.,0.,5.5));
#11752=CARTESIAN_POINT('',(10.2374368670765,1.23743686707646,4.7));
#11753=CARTESIAN_POINT('',(7.76256313292354,1.23743686707646,4.7));
#11754=CARTESIAN_POINT('',(7.76256313292354,-1.23743686707646,4.7));
#11755=CARTESIAN_POINT('',(10.2374368670765,-1.23743686707646,4.7));
#11756=CARTESIAN_POINT('',(10.2374368670765,1.23743686707646,6.3));
#11757=CARTESIAN_POINT('',(7.76256313292354,1.23743686707646,6.3));
#11758=CARTESIAN_POINT('',(7.76256313292354,-1.23743686707646,6.3));
#11759=CARTESIAN_POINT('',(10.2374368670765,-1.23743686707646,6.3));
#11760=CARTESIAN_POINT('',(0.,0.,0.));
#11761=CARTESIAN_POINT('',(0.,0.,0.));
#11762=CARTESIAN_POINT('Origin',(9.,0.,7.9));
#11763=CARTESIAN_POINT('',(8.835,-2.02066721859312E-17,7.9));
#11764=CARTESIAN_POINT('Origin',(9.,0.,7.9));
#11765=CARTESIAN_POINT('',(8.835,2.02066721859312E-17,9.));
#11766=CARTESIAN_POINT('',(8.835,-2.02066721859312E-17,7.9));
#11767=CARTESIAN_POINT('Origin',(9.,0.,9.));
#11768=CARTESIAN_POINT('Origin',(9.,0.,7.9));
#11769=CARTESIAN_POINT('Origin',(9.,0.,7.));
#11770=CARTESIAN_POINT('',(8.6,-4.89858719658942E-17,9.));
#11771=CARTESIAN_POINT('Origin',(9.,0.,9.));
#11772=CARTESIAN_POINT('',(8.6,-4.89858719658942E-17,7.));
#11773=CARTESIAN_POINT('',(8.6,-4.89858719658942E-17,7.));
#11774=CARTESIAN_POINT('Origin',(9.,0.,7.));
#11775=CARTESIAN_POINT('Origin',(9.,0.,9.));
#11776=CARTESIAN_POINT('Origin',(9.,0.,5.95));
#11777=CARTESIAN_POINT('',(8.3,-8.57252759403146E-17,5.95));
#11778=CARTESIAN_POINT('Origin',(9.,0.,5.95));
#11779=CARTESIAN_POINT('',(8.5,6.12323399573677E-17,5.95));
#11780=CARTESIAN_POINT('Origin',(9.,0.,5.95));
#11781=CARTESIAN_POINT('Origin',(9.,0.,5.95));
#11782=CARTESIAN_POINT('',(8.3,-8.57252759403146E-17,7.));
#11783=CARTESIAN_POINT('Origin',(9.,0.,7.));
#11784=CARTESIAN_POINT('',(8.3,-8.57252759403146E-17,5.95));
#11785=CARTESIAN_POINT('Origin',(9.,0.,4.25));
#11786=CARTESIAN_POINT('',(8.5,-6.12323399573677E-17,4.25));
#11787=CARTESIAN_POINT('',(8.5,-6.12323399573677E-17,4.25));
#11788=CARTESIAN_POINT('Origin',(9.,0.,4.25));
#11789=CARTESIAN_POINT('Origin',(9.,0.,7.));
#11790=CARTESIAN_POINT('Origin',(9.,0.,4.25));
#11791=CARTESIAN_POINT('',(0.,0.,0.));
#11792=CARTESIAN_POINT('Origin',(9.49,0.,4.65));
#11793=CARTESIAN_POINT('',(9.49,0.122167917228709,4.53909463493591));
#11794=CARTESIAN_POINT('',(9.49,0.122167917228709,4.76090536506409));
#11795=CARTESIAN_POINT('',(9.49,0.122167917228709,4.25));
#11796=CARTESIAN_POINT('Origin',(9.49,0.,4.65));
#11797=CARTESIAN_POINT('Origin',(9.49,0.,4.65));
#11798=CARTESIAN_POINT('',(9.49,-0.122167917228709,4.53909463493591));
#11799=CARTESIAN_POINT('Ctrl Pts',(9.49,-0.122167917228708,4.53909463493591));
#11800=CARTESIAN_POINT('Ctrl Pts',(9.49044853167999,-0.120368913626297,
4.53711294069536));
#11801=CARTESIAN_POINT('Ctrl Pts',(9.49089524537169,-0.118534896565231,
4.53518965877367));
#11802=CARTESIAN_POINT('Ctrl Pts',(9.49479501553165,-0.102111993019358,
4.5187667552278));
#11803=CARTESIAN_POINT('Ctrl Pts',(9.49844251460759,-0.0836597150224316,
4.50609154388858));
#11804=CARTESIAN_POINT('Ctrl Pts',(9.50357781976106,-0.0430495960471595,
4.48920409039234));
#11805=CARTESIAN_POINT('Ctrl Pts',(9.505,-0.020880094330741,4.485));
#11806=CARTESIAN_POINT('Ctrl Pts',(9.505,0.020880094330741,4.485));
#11807=CARTESIAN_POINT('Ctrl Pts',(9.50357781976106,0.0430495960471595,
4.48920409039234));
#11808=CARTESIAN_POINT('Ctrl Pts',(9.49844251460759,0.0836597150224316,
4.50609154388858));
#11809=CARTESIAN_POINT('Ctrl Pts',(9.49479501553165,0.102111993019358,4.5187667552278));
#11810=CARTESIAN_POINT('Ctrl Pts',(9.49089524537169,0.118534896565231,4.53518965877367));
#11811=CARTESIAN_POINT('Ctrl Pts',(9.49044853167999,0.120368913626297,4.53711294069536));
#11812=CARTESIAN_POINT('Ctrl Pts',(9.49,0.122167917228708,4.53909463493591));
#11813=CARTESIAN_POINT('',(9.49,-0.122167917228709,4.76090536506409));
#11814=CARTESIAN_POINT('Origin',(9.49,0.,4.65));
#11815=CARTESIAN_POINT('',(9.505,-1.70422299968729E-17,4.815));
#11816=CARTESIAN_POINT('Ctrl Pts',(9.505,-2.77555756156289E-17,4.815));
#11817=CARTESIAN_POINT('Ctrl Pts',(9.505,-0.020880094330741,4.815));
#11818=CARTESIAN_POINT('Ctrl Pts',(9.50357781976106,-0.0430495960471595,
4.81079590960766));
#11819=CARTESIAN_POINT('Ctrl Pts',(9.49844251460759,-0.0836597150224317,
4.79390845611142));
#11820=CARTESIAN_POINT('Ctrl Pts',(9.49479501553165,-0.102111993019358,
4.7812332447722));
#11821=CARTESIAN_POINT('Ctrl Pts',(9.49089524537169,-0.118534896565231,
4.76481034122633));
#11822=CARTESIAN_POINT('Ctrl Pts',(9.49044853167999,-0.120368913626296,
4.76288705930464));
#11823=CARTESIAN_POINT('Ctrl Pts',(9.49,-0.122167917228708,4.76090536506409));
#11824=CARTESIAN_POINT('',(9.9,-2.02066721859313E-17,4.815));
#11825=CARTESIAN_POINT('',(9.49,-2.02066721859313E-17,4.815));
#11826=CARTESIAN_POINT('',(9.88474572618352,0.165,4.65));
#11827=CARTESIAN_POINT('Ctrl Pts',(9.88474572618352,0.165,4.65));
#11828=CARTESIAN_POINT('Ctrl Pts',(9.88474572618352,0.165,4.62923124059256));
#11829=CARTESIAN_POINT('Ctrl Pts',(9.88555275950526,0.160839719007584,4.60711110492666));
#11830=CARTESIAN_POINT('Ctrl Pts',(9.88844864815004,0.14398647021669,4.56647293736623));
#11831=CARTESIAN_POINT('Ctrl Pts',(9.89049360485164,0.131295993814186,4.54795075602263));
#11832=CARTESIAN_POINT('Ctrl Pts',(9.89431723432394,0.102049819008125,4.51870458121656));
#11833=CARTESIAN_POINT('Ctrl Pts',(9.89634708889954,0.0835273920906821,
4.50601365401642));
#11834=CARTESIAN_POINT('Ctrl Pts',(9.89920827186059,0.0428883760934128,
4.48916007816136));
#11835=CARTESIAN_POINT('Ctrl Pts',(9.9,0.0207679427235068,4.485));
#11836=CARTESIAN_POINT('Ctrl Pts',(9.9,-0.0207679427235068,4.485));
#11837=CARTESIAN_POINT('Ctrl Pts',(9.89920827186059,-0.0428883760934128,
4.48916007816136));
#11838=CARTESIAN_POINT('Ctrl Pts',(9.89634708889954,-0.0835273920906821,
4.50601365401642));
#11839=CARTESIAN_POINT('Ctrl Pts',(9.89431723432394,-0.102049819008125,
4.51870458121656));
#11840=CARTESIAN_POINT('Ctrl Pts',(9.89049360485164,-0.131295993814186,
4.54795075602263));
#11841=CARTESIAN_POINT('Ctrl Pts',(9.88844864815004,-0.14398647021669,4.56647293736623));
#11842=CARTESIAN_POINT('Ctrl Pts',(9.88555275950526,-0.160839719007584,
4.60711110492666));
#11843=CARTESIAN_POINT('Ctrl Pts',(9.88474572618352,-0.165,4.62923124059256));
#11844=CARTESIAN_POINT('Ctrl Pts',(9.88474572618352,-0.165,4.67076875940744));
#11845=CARTESIAN_POINT('Ctrl Pts',(9.88555275950526,-0.160839719007584,
4.69288889507335));
#11846=CARTESIAN_POINT('Ctrl Pts',(9.88844864815004,-0.14398647021669,4.73352706263377));
#11847=CARTESIAN_POINT('Ctrl Pts',(9.89049360485164,-0.131295993814186,
4.75204924397737));
#11848=CARTESIAN_POINT('Ctrl Pts',(9.89431723432394,-0.102049819008125,
4.78129541878344));
#11849=CARTESIAN_POINT('Ctrl Pts',(9.89634708889954,-0.0835273920906821,
4.79398634598358));
#11850=CARTESIAN_POINT('Ctrl Pts',(9.89920827186059,-0.0428883760934128,
4.81083992183864));
#11851=CARTESIAN_POINT('Ctrl Pts',(9.9,-0.0207679427235068,4.815));
#11852=CARTESIAN_POINT('Ctrl Pts',(9.9,0.,4.815));
#11853=CARTESIAN_POINT('Ctrl Pts',(9.9,-2.08166817117217E-17,4.815));
#11854=CARTESIAN_POINT('Ctrl Pts',(9.9,0.0207679427235068,4.815));
#11855=CARTESIAN_POINT('Ctrl Pts',(9.89920827186059,0.0428883760934128,
4.81083992183864));
#11856=CARTESIAN_POINT('Ctrl Pts',(9.89634708889954,0.0835273920906821,
4.79398634598358));
#11857=CARTESIAN_POINT('Ctrl Pts',(9.89431723432394,0.102049819008125,4.78129541878344));
#11858=CARTESIAN_POINT('Ctrl Pts',(9.89049360485164,0.131295993814186,4.75204924397737));
#11859=CARTESIAN_POINT('Ctrl Pts',(9.88844864815004,0.14398647021669,4.73352706263377));
#11860=CARTESIAN_POINT('Ctrl Pts',(9.88555275950526,0.160839719007584,4.69288889507335));
#11861=CARTESIAN_POINT('Ctrl Pts',(9.88474572618352,0.165,4.67076875940744));
#11862=CARTESIAN_POINT('Ctrl Pts',(9.88474572618352,0.165,4.65));
#11863=CARTESIAN_POINT('Ctrl Pts',(9.49,0.122167917228708,4.76090536506409));
#11864=CARTESIAN_POINT('Ctrl Pts',(9.49044853167999,0.120368913626296,4.76288705930464));
#11865=CARTESIAN_POINT('Ctrl Pts',(9.49089524537169,0.118534896565231,4.76481034122633));
#11866=CARTESIAN_POINT('Ctrl Pts',(9.49479501553165,0.102111993019358,4.7812332447722));
#11867=CARTESIAN_POINT('Ctrl Pts',(9.49844251460759,0.0836597150224316,
4.79390845611142));
#11868=CARTESIAN_POINT('Ctrl Pts',(9.50357781976106,0.0430495960471595,
4.81079590960766));
#11869=CARTESIAN_POINT('Ctrl Pts',(9.505,0.020880094330741,4.815));
#11870=CARTESIAN_POINT('Ctrl Pts',(9.505,-2.77555756156289E-17,4.815));
#11871=CARTESIAN_POINT('Origin',(9.49,0.,4.65));
#11872=CARTESIAN_POINT('',(9.49,-0.122167917228709,4.25));
#11873=CARTESIAN_POINT('Origin',(9.,0.,4.25));
#11874=CARTESIAN_POINT('',(8.495,-6.18446633569414E-17,5.05));
#11875=CARTESIAN_POINT('Origin',(9.,0.,5.05));
#11876=CARTESIAN_POINT('',(8.495,-6.18446633569414E-17,4.25));
#11877=CARTESIAN_POINT('',(8.495,-6.18446633569414E-17,4.25));
#11878=CARTESIAN_POINT('Origin',(9.,0.,4.25));
#11879=CARTESIAN_POINT('Origin',(9.,0.,4.25));
#11880=CARTESIAN_POINT('',(8.1,-1.10218211923262E-16,5.05));
#11881=CARTESIAN_POINT('Origin',(9.,0.,5.05));
#11882=CARTESIAN_POINT('',(8.1,-1.10218211923262E-16,4.25));
#11883=CARTESIAN_POINT('',(8.1,-1.10218211923262E-16,4.25));
#11884=CARTESIAN_POINT('Origin',(9.,0.,4.25));
#11885=CARTESIAN_POINT('Origin',(9.,0.,5.05));
#11886=CARTESIAN_POINT('Origin',(9.,0.,4.25));
#11887=CARTESIAN_POINT('',(0.,0.,0.));
#11888=CARTESIAN_POINT('Origin',(9.,0.,7.));
#11889=CARTESIAN_POINT('',(8.595,-4.95981953654677E-17,7.2));
#11890=CARTESIAN_POINT('Origin',(9.,0.,7.2));
#11891=CARTESIAN_POINT('',(8.595,-4.95981953654677E-17,7.));
#11892=CARTESIAN_POINT('',(8.595,-4.95981953654677E-17,7.));
#11893=CARTESIAN_POINT('Origin',(9.,0.,7.));
#11894=CARTESIAN_POINT('Origin',(9.,0.,7.));
#11895=CARTESIAN_POINT('',(8.4,-7.34788079488412E-17,7.2));
#11896=CARTESIAN_POINT('Origin',(9.,0.,7.2));
#11897=CARTESIAN_POINT('',(8.4,-7.34788079488412E-17,7.));
#11898=CARTESIAN_POINT('',(8.4,-7.34788079488412E-17,7.));
#11899=CARTESIAN_POINT('Origin',(9.,0.,7.));
#11900=CARTESIAN_POINT('Origin',(9.,0.,7.2));
#11901=CARTESIAN_POINT('Origin',(9.,0.,7.));
#11902=CARTESIAN_POINT('',(0.,0.,0.));
#11903=CARTESIAN_POINT('Origin',(9.,0.,8.85));
#11904=CARTESIAN_POINT('',(8.595,-4.95981953654677E-17,9.));
#11905=CARTESIAN_POINT('Origin',(9.,0.,9.));
#11906=CARTESIAN_POINT('',(8.595,-4.95981953654677E-17,8.85));
#11907=CARTESIAN_POINT('',(8.595,-4.95981953654677E-17,8.85));
#11908=CARTESIAN_POINT('Origin',(9.,0.,8.85));
#11909=CARTESIAN_POINT('Origin',(9.,0.,8.85));
#11910=CARTESIAN_POINT('',(8.4,-7.34788079488412E-17,9.));
#11911=CARTESIAN_POINT('Origin',(9.,0.,9.));
#11912=CARTESIAN_POINT('',(8.4,-7.34788079488412E-17,8.85));
#11913=CARTESIAN_POINT('',(8.4,-7.34788079488412E-17,8.85));
#11914=CARTESIAN_POINT('Origin',(9.,0.,8.85));
#11915=CARTESIAN_POINT('Origin',(9.,0.,9.));
#11916=CARTESIAN_POINT('Origin',(9.,0.,8.85));
#11917=CARTESIAN_POINT('',(0.,0.,0.));
#11918=CARTESIAN_POINT('Origin',(8.35,0.,7.55));
#11919=CARTESIAN_POINT('',(8.6,-1.83697019872103E-17,7.7));
#11920=CARTESIAN_POINT('Origin',(8.6,0.,7.55));
#11921=CARTESIAN_POINT('',(8.35,-1.83697019872103E-17,7.7));
#11922=CARTESIAN_POINT('',(8.35,-1.83697019872103E-17,7.7));
#11923=CARTESIAN_POINT('Origin',(8.35,0.,7.55));
#11924=CARTESIAN_POINT('Origin',(8.6,0.,7.55));
#11925=CARTESIAN_POINT('Origin',(8.35,0.,7.55));
#11926=CARTESIAN_POINT('',(0.,0.,0.));
#11927=CARTESIAN_POINT('Origin',(9.4,0.,7.55));
#11928=CARTESIAN_POINT('',(9.65,-1.83697019872103E-17,7.7));
#11929=CARTESIAN_POINT('Origin',(9.65,0.,7.55));
#11930=CARTESIAN_POINT('',(9.4,-1.83697019872103E-17,7.7));
#11931=CARTESIAN_POINT('',(9.4,-1.83697019872103E-17,7.7));
#11932=CARTESIAN_POINT('Origin',(9.4,0.,7.55));
#11933=CARTESIAN_POINT('Origin',(9.65,0.,7.55));
#11934=CARTESIAN_POINT('Origin',(9.4,0.,7.55));
#11935=CARTESIAN_POINT('',(0.,0.,0.));
#11936=CARTESIAN_POINT('Origin',(9.,0.,9.));
#11937=CARTESIAN_POINT('',(8.775,-2.75545529808154E-17,9.2));
#11938=CARTESIAN_POINT('Origin',(9.,0.,9.2));
#11939=CARTESIAN_POINT('',(8.775,-2.75545529808154E-17,9.));
#11940=CARTESIAN_POINT('',(8.775,-2.75545529808154E-17,9.));
#11941=CARTESIAN_POINT('Origin',(9.,0.,9.));
#11942=CARTESIAN_POINT('Origin',(9.,0.,9.));
#11943=CARTESIAN_POINT('',(8.4,-7.34788079488412E-17,9.2));
#11944=CARTESIAN_POINT('Origin',(9.,0.,9.2));
#11945=CARTESIAN_POINT('',(8.4,-7.34788079488412E-17,9.));
#11946=CARTESIAN_POINT('',(8.4,-7.34788079488412E-17,9.));
#11947=CARTESIAN_POINT('Origin',(9.,0.,9.));
#11948=CARTESIAN_POINT('Origin',(9.,0.,9.2));
#11949=CARTESIAN_POINT('Origin',(9.,0.,9.));
#11950=CARTESIAN_POINT('',(0.,0.,0.));
#11951=CARTESIAN_POINT('Origin',(0.,-0.4,0.));
#11952=CARTESIAN_POINT('',(-0.1954,-0.4,2.39295984553393E-17));
#11953=CARTESIAN_POINT('Origin',(0.,-0.4,0.));
#11954=CARTESIAN_POINT('Origin',(0.0577350269189626,0.,-0.1));
#11955=CARTESIAN_POINT('',(0.0577350269189626,0.,-0.1));
#11956=CARTESIAN_POINT('',(0.115470053837925,0.,0.));
#11957=CARTESIAN_POINT('',(0.0934187836487032,0.,-0.0381939203391614));
#11958=CARTESIAN_POINT('',(0.0577350269189626,-0.2,-0.1));
#11959=CARTESIAN_POINT('',(0.0577350269189626,0.,-0.1));
#11960=CARTESIAN_POINT('',(0.115470053837925,-0.2,0.));
#11961=CARTESIAN_POINT('',(0.115470053837925,-0.2,0.));
#11962=CARTESIAN_POINT('',(0.115470053837925,0.,0.));
#11963=CARTESIAN_POINT('Origin',(-0.0577350269189626,0.,-0.1));
#11964=CARTESIAN_POINT('',(-0.0577350269189626,0.,-0.1));
#11965=CARTESIAN_POINT('',(0.0561324865405187,0.,-0.1));
#11966=CARTESIAN_POINT('',(-0.0577350269189626,-0.2,-0.1));
#11967=CARTESIAN_POINT('',(-0.0577350269189626,0.,-0.1));
#11968=CARTESIAN_POINT('',(0.0577350269189626,-0.2,-0.1));
#11969=CARTESIAN_POINT('Origin',(-0.115470053837925,0.,-1.38777878078145E-17));
#11970=CARTESIAN_POINT('',(-0.115470053837925,0.,-1.41410031829988E-17));
#11971=CARTESIAN_POINT('',(-0.0797862971081845,0.,-0.0618060796608387));
#11972=CARTESIAN_POINT('',(-0.115470053837925,-0.2,-1.38777878078145E-17));
#11973=CARTESIAN_POINT('',(-0.115470053837925,0.,-1.41410031829988E-17));
#11974=CARTESIAN_POINT('',(-0.0577350269189626,-0.2,-0.1));
#11975=CARTESIAN_POINT('Origin',(-0.0577350269189626,0.,0.1));
#11976=CARTESIAN_POINT('',(-0.0577350269189626,0.,0.1));
#11977=CARTESIAN_POINT('',(-0.0509187836487033,0.,0.111806079660839));
#11978=CARTESIAN_POINT('',(-0.0577350269189626,-0.2,0.1));
#11979=CARTESIAN_POINT('',(-0.0577350269189626,0.,0.1));
#11980=CARTESIAN_POINT('',(-0.115470053837925,-0.2,-1.41410031829988E-17));
#11981=CARTESIAN_POINT('Origin',(0.0577350269189626,0.,0.1));
#11982=CARTESIAN_POINT('',(0.0577350269189626,0.,0.1));
#11983=CARTESIAN_POINT('',(0.113867513459481,0.,0.1));
#11984=CARTESIAN_POINT('',(0.0577350269189626,-0.2,0.1));
#11985=CARTESIAN_POINT('',(0.0577350269189626,0.,0.1));
#11986=CARTESIAN_POINT('',(-0.0577350269189626,-0.2,0.1));
#11987=CARTESIAN_POINT('Origin',(0.115470053837925,0.,0.));
#11988=CARTESIAN_POINT('',(0.122286297108185,0.,-0.0118060796608386));
#11989=CARTESIAN_POINT('',(0.0577350269189626,-0.2,0.1));
#11990=CARTESIAN_POINT('Origin',(0.,-0.2,0.));
#11991=CARTESIAN_POINT('Origin',(0.17,0.,0.));
#11992=CARTESIAN_POINT('',(-0.17,-8.67361737988404E-18,-2.0818995585505E-17));
#11993=CARTESIAN_POINT('Origin',(0.,0.,0.));
#11994=CARTESIAN_POINT('Origin',(0.,-0.015,0.));
#11995=CARTESIAN_POINT('',(-0.1954,-0.0254,-2.39295984553393E-17));
#11996=CARTESIAN_POINT('Origin',(0.,-0.0254,0.));
#11997=CARTESIAN_POINT('',(-0.185,-0.015,-2.2655965784226E-17));
#11998=CARTESIAN_POINT('Origin',(0.,-0.2775,0.));
#11999=CARTESIAN_POINT('',(-0.1954,-0.2775,-2.39295984553393E-17));
#12000=CARTESIAN_POINT('',(0.,0.,0.));
#12001=CARTESIAN_POINT('',(0.,0.,0.));
#12002=CARTESIAN_POINT('',(0.,0.,0.));
#12003=CARTESIAN_POINT('',(0.,0.,0.));
#12004=CARTESIAN_POINT('',(0.,0.,0.));
#12005=CARTESIAN_POINT('',(0.,0.,0.));
#12006=CARTESIAN_POINT('',(0.,0.,0.));
#12007=CARTESIAN_POINT('',(0.,0.,0.));
#12008=CARTESIAN_POINT('',(2.2,0.,0.8));
#12009=CARTESIAN_POINT('',(2.2,0.,0.9));
#12010=CARTESIAN_POINT('',(-1.1,1.90525588832577,0.8));
#12011=CARTESIAN_POINT('',(-1.1,1.90525588832577,0.9));
#12012=CARTESIAN_POINT('',(-1.1,-1.90525588832576,0.8));
#12013=CARTESIAN_POINT('',(-1.1,-1.90525588832576,0.9));
#12014=CARTESIAN_POINT('',(0.9,0.,6.35));
#12015=CARTESIAN_POINT('',(0.8,-3.5,-1.));
#12016=CARTESIAN_POINT('',(6.,2.8,5.5));
#12017=CARTESIAN_POINT('',(6.,2.3,5.5));
#12018=CARTESIAN_POINT('',(6.,1.9,-1.));
#12019=CARTESIAN_POINT('',(0.,0.,0.));
#12020=CARTESIAN_POINT('Origin',(0.,-0.45,0.));
#12021=CARTESIAN_POINT('',(-0.65,-0.325,-3.9801020972289E-17));
#12022=CARTESIAN_POINT('',(-0.637867541108654,-0.45,0.125));
#12023=CARTESIAN_POINT('Ctrl Pts',(-0.65,-0.325,-6.93889390390723E-17));
#12024=CARTESIAN_POINT('Ctrl Pts',(-0.65,-0.325,0.0157371373481997));
#12025=CARTESIAN_POINT('Ctrl Pts',(-0.649370620646074,-0.328153081062251,
0.0324967135411163));
#12026=CARTESIAN_POINT('Ctrl Pts',(-0.647096224417991,-0.340922081922822,
0.0632828231545122));
#12027=CARTESIAN_POINT('Ctrl Pts',(-0.645482573914132,-0.350535859112198,
0.0773125544088347));
#12028=CARTESIAN_POINT('Ctrl Pts',(-0.642442040715078,-0.372687974598127,
0.0994646698947638));
#12029=CARTESIAN_POINT('Ctrl Pts',(-0.640815160902589,-0.386717480603274,
0.109078032552995));
#12030=CARTESIAN_POINT('Ctrl Pts',(-0.63851034608138,-0.417502809542363,
0.121846732641678));
#12031=CARTESIAN_POINT('Ctrl Pts',(-0.637867541108654,-0.434262111007648,
0.125));
#12032=CARTESIAN_POINT('Ctrl Pts',(-0.637867541108654,-0.45,0.125));
#12033=CARTESIAN_POINT('',(-0.65,-0.575,-3.9801020972289E-17));
#12034=CARTESIAN_POINT('Ctrl Pts',(-0.65,-0.575,-3.46944695195361E-18));
#12035=CARTESIAN_POINT('Ctrl Pts',(-0.65,-0.575,-0.0157371373481998));
#12036=CARTESIAN_POINT('Ctrl Pts',(-0.649370620646074,-0.571846918937749,
-0.0324967135411164));
#12037=CARTESIAN_POINT('Ctrl Pts',(-0.647096224417991,-0.559077918077178,
-0.0632828231545123));
#12038=CARTESIAN_POINT('Ctrl Pts',(-0.645482573914132,-0.549464140887802,
-0.0773125544088349));
#12039=CARTESIAN_POINT('Ctrl Pts',(-0.642442040715078,-0.527312025401873,
-0.099464669894764));
#12040=CARTESIAN_POINT('Ctrl Pts',(-0.640815160902589,-0.513282519396725,
-0.109078032552995));
#12041=CARTESIAN_POINT('Ctrl Pts',(-0.63851034608138,-0.482497190457637,
-0.121846732641678));
#12042=CARTESIAN_POINT('Ctrl Pts',(-0.637867541108654,-0.465737888992352,
-0.125));
#12043=CARTESIAN_POINT('Ctrl Pts',(-0.637867541108654,-0.434262111007648,
-0.125));
#12044=CARTESIAN_POINT('Ctrl Pts',(-0.63851034608138,-0.417502809542363,
-0.121846732641678));
#12045=CARTESIAN_POINT('Ctrl Pts',(-0.640815160902589,-0.386717480603275,
-0.109078032552995));
#12046=CARTESIAN_POINT('Ctrl Pts',(-0.642442040715078,-0.372687974598127,
-0.099464669894764));
#12047=CARTESIAN_POINT('Ctrl Pts',(-0.645482573914132,-0.350535859112198,
-0.077312554408835));
#12048=CARTESIAN_POINT('Ctrl Pts',(-0.647096224417991,-0.340922081922822,
-0.0632828231545124));
#12049=CARTESIAN_POINT('Ctrl Pts',(-0.649370620646074,-0.328153081062251,
-0.0324967135411165));
#12050=CARTESIAN_POINT('Ctrl Pts',(-0.65,-0.325,-0.0157371373481999));
#12051=CARTESIAN_POINT('Ctrl Pts',(-0.65,-0.325,-8.32667268468867E-17));
#12052=CARTESIAN_POINT('Ctrl Pts',(-0.637867541108654,-0.45,0.125));
#12053=CARTESIAN_POINT('Ctrl Pts',(-0.637867541108654,-0.465737888992352,
0.125));
#12054=CARTESIAN_POINT('Ctrl Pts',(-0.63851034608138,-0.482497190457637,
0.121846732641678));
#12055=CARTESIAN_POINT('Ctrl Pts',(-0.640815160902589,-0.513282519396725,
0.109078032552995));
#12056=CARTESIAN_POINT('Ctrl Pts',(-0.642442040715078,-0.527312025401873,
0.0994646698947639));
#12057=CARTESIAN_POINT('Ctrl Pts',(-0.645482573914132,-0.549464140887802,
0.0773125544088349));
#12058=CARTESIAN_POINT('Ctrl Pts',(-0.647096224417991,-0.559077918077178,
0.0632828231545123));
#12059=CARTESIAN_POINT('Ctrl Pts',(-0.649370620646074,-0.571846918937749,
0.0324967135411164));
#12060=CARTESIAN_POINT('Ctrl Pts',(-0.65,-0.575,0.0157371373481998));
#12061=CARTESIAN_POINT('Ctrl Pts',(-0.65,-0.575,-2.08166817117217E-17));
#12062=CARTESIAN_POINT('',(-0.379967103839267,-0.45,0.125));
#12063=CARTESIAN_POINT('',(-7.65404249467096E-18,-0.45,0.125));
#12064=CARTESIAN_POINT('',(-0.4,-0.575,5.41097774720219E-18));
#12065=CARTESIAN_POINT('Ctrl Pts',(-0.4,-0.575,-3.81639164714898E-17));
#12066=CARTESIAN_POINT('Ctrl Pts',(-0.4,-0.575,0.0158075115832675));
#12067=CARTESIAN_POINT('Ctrl Pts',(-0.398970551469948,-0.571819306519379,
0.0325978607437828));
#12068=CARTESIAN_POINT('Ctrl Pts',(-0.395252954914593,-0.559029081159106,
0.0633657881355917));
#12069=CARTESIAN_POINT('Ctrl Pts',(-0.392612801026882,-0.549425200318011,
0.0773514949786256));
#12070=CARTESIAN_POINT('Ctrl Pts',(-0.38761064154154,-0.527347592689753,
0.0994291026068839));
#12071=CARTESIAN_POINT('Ctrl Pts',(-0.384911758361269,-0.51336346023721,
0.109029967924066));
#12072=CARTESIAN_POINT('Ctrl Pts',(-0.381057715344782,-0.48260129709332,
0.121817958968287));
#12073=CARTESIAN_POINT('Ctrl Pts',(-0.379967103839267,-0.465813100629203,
0.125));
#12074=CARTESIAN_POINT('Ctrl Pts',(-0.379967103839267,-0.45,0.125));
#12075=CARTESIAN_POINT('',(-0.379967103839267,-0.45,-0.125));
#12076=CARTESIAN_POINT('Ctrl Pts',(-0.379967103839267,-0.45,-0.125));
#12077=CARTESIAN_POINT('Ctrl Pts',(-0.379967103839267,-0.465813100629203,
-0.125));
#12078=CARTESIAN_POINT('Ctrl Pts',(-0.381057715344782,-0.48260129709332,
-0.121817958968287));
#12079=CARTESIAN_POINT('Ctrl Pts',(-0.384911758361269,-0.51336346023721,
-0.109029967924066));
#12080=CARTESIAN_POINT('Ctrl Pts',(-0.38761064154154,-0.527347592689753,
-0.099429102606884));
#12081=CARTESIAN_POINT('Ctrl Pts',(-0.392612801026882,-0.549425200318011,
-0.0773514949786257));
#12082=CARTESIAN_POINT('Ctrl Pts',(-0.395252954914593,-0.559029081159106,
-0.0633657881355918));
#12083=CARTESIAN_POINT('Ctrl Pts',(-0.398970551469948,-0.571819306519379,
-0.0325978607437828));
#12084=CARTESIAN_POINT('Ctrl Pts',(-0.4,-0.575,-0.0158075115832676));
#12085=CARTESIAN_POINT('Ctrl Pts',(-0.4,-0.575,-4.16333634234434E-17));
#12086=CARTESIAN_POINT('',(-0.4,-0.325,2.96971064108775E-17));
#12087=CARTESIAN_POINT('Ctrl Pts',(-0.4,-0.325,1.04083408558608E-17));
#12088=CARTESIAN_POINT('Ctrl Pts',(-0.4,-0.325,-0.0158075115832676));
#12089=CARTESIAN_POINT('Ctrl Pts',(-0.398970551469948,-0.328180693480621,
-0.0325978607437828));
#12090=CARTESIAN_POINT('Ctrl Pts',(-0.395252954914593,-0.340970918840894,
-0.0633657881355918));
#12091=CARTESIAN_POINT('Ctrl Pts',(-0.392612801026882,-0.350574799681989,
-0.0773514949786256));
#12092=CARTESIAN_POINT('Ctrl Pts',(-0.38761064154154,-0.372652407310247,
-0.0994291026068839));
#12093=CARTESIAN_POINT('Ctrl Pts',(-0.384911758361269,-0.38663653976279,
-0.109029967924066));
#12094=CARTESIAN_POINT('Ctrl Pts',(-0.381057715344782,-0.41739870290668,
-0.121817958968287));
#12095=CARTESIAN_POINT('Ctrl Pts',(-0.379967103839267,-0.434186899370797,
-0.125));
#12096=CARTESIAN_POINT('Ctrl Pts',(-0.379967103839267,-0.45,-0.125));
#12097=CARTESIAN_POINT('Ctrl Pts',(-0.379967103839267,-0.45,0.125));
#12098=CARTESIAN_POINT('Ctrl Pts',(-0.379967103839267,-0.434186899370797,
0.125));
#12099=CARTESIAN_POINT('Ctrl Pts',(-0.381057715344782,-0.41739870290668,
0.121817958968287));
#12100=CARTESIAN_POINT('Ctrl Pts',(-0.384911758361269,-0.38663653976279,
0.109029967924066));
#12101=CARTESIAN_POINT('Ctrl Pts',(-0.38761064154154,-0.372652407310247,
0.0994291026068839));
#12102=CARTESIAN_POINT('Ctrl Pts',(-0.392612801026882,-0.350574799681989,
0.0773514949786257));
#12103=CARTESIAN_POINT('Ctrl Pts',(-0.395252954914593,-0.340970918840894,
0.0633657881355918));
#12104=CARTESIAN_POINT('Ctrl Pts',(-0.398970551469948,-0.328180693480621,
0.0325978607437829));
#12105=CARTESIAN_POINT('Ctrl Pts',(-0.4,-0.325,0.0158075115832676));
#12106=CARTESIAN_POINT('Ctrl Pts',(-0.4,-0.325,1.38777878078145E-17));
#12107=CARTESIAN_POINT('Origin',(0.,-0.45,0.));
#12108=CARTESIAN_POINT('',(0.379967103839267,-0.45,-0.125));
#12109=CARTESIAN_POINT('',(0.379967103839267,-0.45,0.125));
#12110=CARTESIAN_POINT('Ctrl Pts',(0.379967103839267,-0.45,-0.125));
#12111=CARTESIAN_POINT('Ctrl Pts',(0.379967103839267,-0.434186899370797,
-0.125));
#12112=CARTESIAN_POINT('Ctrl Pts',(0.381057715344782,-0.41739870290668,
-0.121817958968287));
#12113=CARTESIAN_POINT('Ctrl Pts',(0.384911758361269,-0.38663653976279,
-0.109029967924066));
#12114=CARTESIAN_POINT('Ctrl Pts',(0.38761064154154,-0.372652407310247,
-0.0994291026068839));
#12115=CARTESIAN_POINT('Ctrl Pts',(0.392612801026882,-0.350574799681989,
-0.0773514949786256));
#12116=CARTESIAN_POINT('Ctrl Pts',(0.395252954914593,-0.340970918840894,
-0.0633657881355917));
#12117=CARTESIAN_POINT('Ctrl Pts',(0.398970551469948,-0.328180693480621,
-0.0325978607437828));
#12118=CARTESIAN_POINT('Ctrl Pts',(0.4,-0.325,-0.0158075115832675));
#12119=CARTESIAN_POINT('Ctrl Pts',(0.4,-0.325,0.0158075115832676));
#12120=CARTESIAN_POINT('Ctrl Pts',(0.398970551469948,-0.328180693480621,
0.0325978607437829));
#12121=CARTESIAN_POINT('Ctrl Pts',(0.395252954914593,-0.340970918840894,
0.0633657881355918));
#12122=CARTESIAN_POINT('Ctrl Pts',(0.392612801026882,-0.350574799681989,
0.0773514949786257));
#12123=CARTESIAN_POINT('Ctrl Pts',(0.38761064154154,-0.372652407310247,
0.099429102606884));
#12124=CARTESIAN_POINT('Ctrl Pts',(0.384911758361269,-0.38663653976279,
0.109029967924066));
#12125=CARTESIAN_POINT('Ctrl Pts',(0.381057715344782,-0.41739870290668,
0.121817958968287));
#12126=CARTESIAN_POINT('Ctrl Pts',(0.379967103839267,-0.434186899370797,
0.125));
#12127=CARTESIAN_POINT('Ctrl Pts',(0.379967103839267,-0.45,0.125));
#12128=CARTESIAN_POINT('Ctrl Pts',(0.379967103839267,-0.45,0.125));
#12129=CARTESIAN_POINT('Ctrl Pts',(0.379967103839267,-0.465813100629203,
0.125));
#12130=CARTESIAN_POINT('Ctrl Pts',(0.381057715344782,-0.48260129709332,
0.121817958968287));
#12131=CARTESIAN_POINT('Ctrl Pts',(0.384911758361269,-0.51336346023721,
0.109029967924066));
#12132=CARTESIAN_POINT('Ctrl Pts',(0.38761064154154,-0.527347592689753,
0.0994291026068839));
#12133=CARTESIAN_POINT('Ctrl Pts',(0.392612801026882,-0.549425200318011,
0.0773514949786257));
#12134=CARTESIAN_POINT('Ctrl Pts',(0.395252954914593,-0.559029081159106,
0.0633657881355918));
#12135=CARTESIAN_POINT('Ctrl Pts',(0.398970551469948,-0.571819306519379,
0.0325978607437829));
#12136=CARTESIAN_POINT('Ctrl Pts',(0.4,-0.575,0.0158075115832676));
#12137=CARTESIAN_POINT('Ctrl Pts',(0.4,-0.575,-0.0158075115832676));
#12138=CARTESIAN_POINT('Ctrl Pts',(0.398970551469948,-0.57181930651938,
-0.0325978607437828));
#12139=CARTESIAN_POINT('Ctrl Pts',(0.395252954914593,-0.559029081159106,
-0.0633657881355918));
#12140=CARTESIAN_POINT('Ctrl Pts',(0.392612801026882,-0.549425200318011,
-0.0773514949786257));
#12141=CARTESIAN_POINT('Ctrl Pts',(0.38761064154154,-0.527347592689753,
-0.0994291026068839));
#12142=CARTESIAN_POINT('Ctrl Pts',(0.384911758361269,-0.51336346023721,
-0.109029967924066));
#12143=CARTESIAN_POINT('Ctrl Pts',(0.381057715344782,-0.48260129709332,
-0.121817958968287));
#12144=CARTESIAN_POINT('Ctrl Pts',(0.379967103839267,-0.465813100629203,
-0.125));
#12145=CARTESIAN_POINT('Ctrl Pts',(0.379967103839267,-0.45,-0.125));
#12146=CARTESIAN_POINT('',(0.637867541108654,-0.45,0.125));
#12147=CARTESIAN_POINT('',(-7.65404249467096E-18,-0.45,0.125));
#12148=CARTESIAN_POINT('',(0.65,-0.575,3.9801020972289E-17));
#12149=CARTESIAN_POINT('Ctrl Pts',(0.65,-0.575,5.55111512312578E-17));
#12150=CARTESIAN_POINT('Ctrl Pts',(0.65,-0.575,0.0157371373481999));
#12151=CARTESIAN_POINT('Ctrl Pts',(0.649370620646074,-0.571846918937749,
0.0324967135411165));
#12152=CARTESIAN_POINT('Ctrl Pts',(0.647096224417991,-0.559077918077178,
0.0632828231545124));
#12153=CARTESIAN_POINT('Ctrl Pts',(0.645482573914132,-0.549464140887802,
0.077312554408835));
#12154=CARTESIAN_POINT('Ctrl Pts',(0.642442040715078,-0.527312025401873,
0.099464669894764));
#12155=CARTESIAN_POINT('Ctrl Pts',(0.640815160902589,-0.513282519396725,
0.109078032552995));
#12156=CARTESIAN_POINT('Ctrl Pts',(0.63851034608138,-0.482497190457637,
0.121846732641678));
#12157=CARTESIAN_POINT('Ctrl Pts',(0.637867541108654,-0.465737888992352,
0.125));
#12158=CARTESIAN_POINT('Ctrl Pts',(0.637867541108654,-0.45,0.125));
#12159=CARTESIAN_POINT('',(0.65,-0.325,3.9801020972289E-17));
#12160=CARTESIAN_POINT('Ctrl Pts',(0.65,-0.325,6.93889390390723E-18));
#12161=CARTESIAN_POINT('Ctrl Pts',(0.65,-0.325,-0.0157371373481998));
#12162=CARTESIAN_POINT('Ctrl Pts',(0.649370620646074,-0.328153081062251,
-0.0324967135411164));
#12163=CARTESIAN_POINT('Ctrl Pts',(0.647096224417991,-0.340922081922822,
-0.0632828231545123));
#12164=CARTESIAN_POINT('Ctrl Pts',(0.645482573914132,-0.350535859112198,
-0.0773125544088349));
#12165=CARTESIAN_POINT('Ctrl Pts',(0.642442040715078,-0.372687974598127,
-0.0994646698947639));
#12166=CARTESIAN_POINT('Ctrl Pts',(0.640815160902588,-0.386717480603275,
-0.109078032552995));
#12167=CARTESIAN_POINT('Ctrl Pts',(0.63851034608138,-0.417502809542363,
-0.121846732641678));
#12168=CARTESIAN_POINT('Ctrl Pts',(0.637867541108654,-0.434262111007648,
-0.125));
#12169=CARTESIAN_POINT('Ctrl Pts',(0.637867541108654,-0.465737888992352,
-0.125));
#12170=CARTESIAN_POINT('Ctrl Pts',(0.63851034608138,-0.482497190457637,
-0.121846732641678));
#12171=CARTESIAN_POINT('Ctrl Pts',(0.640815160902589,-0.513282519396725,
-0.109078032552995));
#12172=CARTESIAN_POINT('Ctrl Pts',(0.642442040715078,-0.527312025401873,
-0.0994646698947639));
#12173=CARTESIAN_POINT('Ctrl Pts',(0.645482573914132,-0.549464140887802,
-0.0773125544088348));
#12174=CARTESIAN_POINT('Ctrl Pts',(0.647096224417991,-0.559077918077178,
-0.0632828231545123));
#12175=CARTESIAN_POINT('Ctrl Pts',(0.649370620646074,-0.571846918937749,
-0.0324967135411164));
#12176=CARTESIAN_POINT('Ctrl Pts',(0.65,-0.575,-0.0157371373481998));
#12177=CARTESIAN_POINT('Ctrl Pts',(0.65,-0.575,6.24500451351651E-17));
#12178=CARTESIAN_POINT('Ctrl Pts',(0.637867541108654,-0.45,0.125));
#12179=CARTESIAN_POINT('Ctrl Pts',(0.637867541108654,-0.434262111007648,
0.125));
#12180=CARTESIAN_POINT('Ctrl Pts',(0.63851034608138,-0.417502809542363,
0.121846732641678));
#12181=CARTESIAN_POINT('Ctrl Pts',(0.640815160902589,-0.386717480603274,
0.109078032552995));
#12182=CARTESIAN_POINT('Ctrl Pts',(0.642442040715078,-0.372687974598127,
0.0994646698947639));
#12183=CARTESIAN_POINT('Ctrl Pts',(0.645482573914132,-0.350535859112198,
0.0773125544088348));
#12184=CARTESIAN_POINT('Ctrl Pts',(0.647096224417991,-0.340922081922822,
0.0632828231545123));
#12185=CARTESIAN_POINT('Ctrl Pts',(0.649370620646074,-0.328153081062251,
0.0324967135411164));
#12186=CARTESIAN_POINT('Ctrl Pts',(0.65,-0.325,0.0157371373481998));
#12187=CARTESIAN_POINT('Ctrl Pts',(0.65,-0.325,-6.93889390390723E-18));
#12188=CARTESIAN_POINT('Origin',(0.,-0.1,0.));
#12189=CARTESIAN_POINT('',(-0.65,-0.8,7.9602041944578E-17));
#12190=CARTESIAN_POINT('Origin',(0.,-0.8,0.));
#12191=CARTESIAN_POINT('',(-0.65,-0.1,-7.9602041944578E-17));
#12192=CARTESIAN_POINT('',(-0.65,-0.1,7.9602041944578E-17));
#12193=CARTESIAN_POINT('',(-0.65,-0.1,-7.9602041944578E-17));
#12194=CARTESIAN_POINT('Origin',(0.,-0.1,0.));
#12195=CARTESIAN_POINT('',(0.,-0.575,-0.65));
#12196=CARTESIAN_POINT('',(0.,-0.325,-0.65));
#12197=CARTESIAN_POINT('Ctrl Pts',(-1.73472347597681E-17,-0.575,-0.65));
#12198=CARTESIAN_POINT('Ctrl Pts',(0.0157371373481998,-0.575,-0.65));
#12199=CARTESIAN_POINT('Ctrl Pts',(0.0324967135411164,-0.571846918937749,
-0.649370620646074));
#12200=CARTESIAN_POINT('Ctrl Pts',(0.0632828231545123,-0.559077918077178,
-0.647096224417991));
#12201=CARTESIAN_POINT('Ctrl Pts',(0.0773125544088349,-0.549464140887802,
-0.645482573914132));
#12202=CARTESIAN_POINT('Ctrl Pts',(0.099464669894764,-0.527312025401873,
-0.642442040715078));
#12203=CARTESIAN_POINT('Ctrl Pts',(0.109078032552995,-0.513282519396725,
-0.640815160902589));
#12204=CARTESIAN_POINT('Ctrl Pts',(0.121846732641678,-0.482497190457636,
-0.63851034608138));
#12205=CARTESIAN_POINT('Ctrl Pts',(0.125,-0.465737888992352,-0.637867541108654));
#12206=CARTESIAN_POINT('Ctrl Pts',(0.125,-0.434262111007648,-0.637867541108654));
#12207=CARTESIAN_POINT('Ctrl Pts',(0.121846732641678,-0.417502809542364,
-0.63851034608138));
#12208=CARTESIAN_POINT('Ctrl Pts',(0.109078032552995,-0.386717480603275,
-0.640815160902589));
#12209=CARTESIAN_POINT('Ctrl Pts',(0.099464669894764,-0.372687974598127,
-0.642442040715078));
#12210=CARTESIAN_POINT('Ctrl Pts',(0.0773125544088349,-0.350535859112198,
-0.645482573914132));
#12211=CARTESIAN_POINT('Ctrl Pts',(0.0632828231545123,-0.340922081922822,
-0.647096224417991));
#12212=CARTESIAN_POINT('Ctrl Pts',(0.0324967135411164,-0.328153081062251,
-0.649370620646074));
#12213=CARTESIAN_POINT('Ctrl Pts',(0.0157371373481999,-0.325,-0.65));
#12214=CARTESIAN_POINT('Ctrl Pts',(4.5102810375397E-17,-0.325,-0.65));
#12215=CARTESIAN_POINT('',(-0.125,-0.45,-0.637867541108654));
#12216=CARTESIAN_POINT('Ctrl Pts',(4.85722573273506E-17,-0.325,-0.65));
#12217=CARTESIAN_POINT('Ctrl Pts',(-0.0157371373481997,-0.325,-0.65));
#12218=CARTESIAN_POINT('Ctrl Pts',(-0.0324967135411163,-0.328153081062251,
-0.649370620646074));
#12219=CARTESIAN_POINT('Ctrl Pts',(-0.0632828231545122,-0.340922081922822,
-0.647096224417991));
#12220=CARTESIAN_POINT('Ctrl Pts',(-0.0773125544088348,-0.350535859112198,
-0.645482573914132));
#12221=CARTESIAN_POINT('Ctrl Pts',(-0.0994646698947639,-0.372687974598127,
-0.642442040715078));
#12222=CARTESIAN_POINT('Ctrl Pts',(-0.109078032552995,-0.386717480603274,
-0.640815160902589));
#12223=CARTESIAN_POINT('Ctrl Pts',(-0.121846732641678,-0.417502809542363,
-0.63851034608138));
#12224=CARTESIAN_POINT('Ctrl Pts',(-0.125,-0.434262111007648,-0.637867541108654));
#12225=CARTESIAN_POINT('Ctrl Pts',(-0.125,-0.45,-0.637867541108654));
#12226=CARTESIAN_POINT('Ctrl Pts',(-0.125,-0.45,-0.637867541108654));
#12227=CARTESIAN_POINT('Ctrl Pts',(-0.125,-0.465737888992352,-0.637867541108654));
#12228=CARTESIAN_POINT('Ctrl Pts',(-0.121846732641678,-0.482497190457636,
-0.63851034608138));
#12229=CARTESIAN_POINT('Ctrl Pts',(-0.109078032552995,-0.513282519396725,
-0.640815160902589));
#12230=CARTESIAN_POINT('Ctrl Pts',(-0.099464669894764,-0.527312025401873,
-0.642442040715078));
#12231=CARTESIAN_POINT('Ctrl Pts',(-0.0773125544088349,-0.549464140887802,
-0.645482573914132));
#12232=CARTESIAN_POINT('Ctrl Pts',(-0.0632828231545124,-0.559077918077178,
-0.647096224417991));
#12233=CARTESIAN_POINT('Ctrl Pts',(-0.0324967135411165,-0.571846918937749,
-0.649370620646074));
#12234=CARTESIAN_POINT('Ctrl Pts',(-0.0157371373481998,-0.575,-0.65));
#12235=CARTESIAN_POINT('Ctrl Pts',(-1.73472347597681E-17,-0.575,-0.65));
#12236=CARTESIAN_POINT('',(0.,-0.325,0.65));
#12237=CARTESIAN_POINT('',(0.,-0.575,0.65));
#12238=CARTESIAN_POINT('Ctrl Pts',(2.77555756156289E-17,-0.325,0.65));
#12239=CARTESIAN_POINT('Ctrl Pts',(0.0157371373481998,-0.325,0.65));
#12240=CARTESIAN_POINT('Ctrl Pts',(0.0324967135411164,-0.328153081062251,
0.649370620646074));
#12241=CARTESIAN_POINT('Ctrl Pts',(0.0632828231545123,-0.340922081922822,
0.647096224417991));
#12242=CARTESIAN_POINT('Ctrl Pts',(0.0773125544088349,-0.350535859112198,
0.645482573914132));
#12243=CARTESIAN_POINT('Ctrl Pts',(0.099464669894764,-0.372687974598127,
0.642442040715078));
#12244=CARTESIAN_POINT('Ctrl Pts',(0.109078032552995,-0.386717480603275,
0.640815160902589));
#12245=CARTESIAN_POINT('Ctrl Pts',(0.121846732641678,-0.417502809542364,
0.63851034608138));
#12246=CARTESIAN_POINT('Ctrl Pts',(0.125,-0.434262111007648,0.637867541108654));
#12247=CARTESIAN_POINT('Ctrl Pts',(0.125,-0.465737888992352,0.637867541108654));
#12248=CARTESIAN_POINT('Ctrl Pts',(0.121846732641678,-0.482497190457636,
0.63851034608138));
#12249=CARTESIAN_POINT('Ctrl Pts',(0.109078032552995,-0.513282519396725,
0.640815160902589));
#12250=CARTESIAN_POINT('Ctrl Pts',(0.099464669894764,-0.527312025401873,
0.642442040715078));
#12251=CARTESIAN_POINT('Ctrl Pts',(0.077312554408835,-0.549464140887802,
0.645482573914132));
#12252=CARTESIAN_POINT('Ctrl Pts',(0.0632828231545124,-0.559077918077178,
0.647096224417991));
#12253=CARTESIAN_POINT('Ctrl Pts',(0.0324967135411165,-0.571846918937749,
0.649370620646074));
#12254=CARTESIAN_POINT('Ctrl Pts',(0.0157371373481998,-0.575,0.65));
#12255=CARTESIAN_POINT('Ctrl Pts',(-1.38777878078145E-17,-0.575,0.65));
#12256=CARTESIAN_POINT('',(-0.125,-0.45,0.637867541108654));
#12257=CARTESIAN_POINT('Ctrl Pts',(-1.04083408558608E-17,-0.575,0.65));
#12258=CARTESIAN_POINT('Ctrl Pts',(-0.0157371373481998,-0.575,0.65));
#12259=CARTESIAN_POINT('Ctrl Pts',(-0.0324967135411164,-0.571846918937749,
0.649370620646074));
#12260=CARTESIAN_POINT('Ctrl Pts',(-0.0632828231545123,-0.559077918077178,
0.647096224417991));
#12261=CARTESIAN_POINT('Ctrl Pts',(-0.0773125544088349,-0.549464140887802,
0.645482573914132));
#12262=CARTESIAN_POINT('Ctrl Pts',(-0.099464669894764,-0.527312025401873,
0.642442040715078));
#12263=CARTESIAN_POINT('Ctrl Pts',(-0.109078032552995,-0.513282519396725,
0.640815160902589));
#12264=CARTESIAN_POINT('Ctrl Pts',(-0.121846732641678,-0.482497190457636,
0.63851034608138));
#12265=CARTESIAN_POINT('Ctrl Pts',(-0.125,-0.465737888992352,0.637867541108654));
#12266=CARTESIAN_POINT('Ctrl Pts',(-0.125,-0.45,0.637867541108654));
#12267=CARTESIAN_POINT('Ctrl Pts',(-0.125,-0.45,0.637867541108654));
#12268=CARTESIAN_POINT('Ctrl Pts',(-0.125,-0.434262111007648,0.637867541108654));
#12269=CARTESIAN_POINT('Ctrl Pts',(-0.121846732641678,-0.417502809542363,
0.63851034608138));
#12270=CARTESIAN_POINT('Ctrl Pts',(-0.109078032552995,-0.386717480603274,
0.640815160902589));
#12271=CARTESIAN_POINT('Ctrl Pts',(-0.0994646698947639,-0.372687974598127,
0.642442040715078));
#12272=CARTESIAN_POINT('Ctrl Pts',(-0.0773125544088348,-0.350535859112198,
0.645482573914132));
#12273=CARTESIAN_POINT('Ctrl Pts',(-0.0632828231545122,-0.340922081922822,
0.647096224417991));
#12274=CARTESIAN_POINT('Ctrl Pts',(-0.0324967135411163,-0.328153081062251,
0.649370620646074));
#12275=CARTESIAN_POINT('Ctrl Pts',(-0.0157371373481998,-0.325,0.65));
#12276=CARTESIAN_POINT('Ctrl Pts',(4.5102810375397E-17,-0.325,0.65));
#12277=CARTESIAN_POINT('Origin',(0.,-0.45,0.));
#12278=CARTESIAN_POINT('',(-0.125,-0.45,-0.379967103839267));
#12279=CARTESIAN_POINT('',(-0.125,-0.45,0.));
#12280=CARTESIAN_POINT('',(0.125,-0.45,-0.379967103839267));
#12281=CARTESIAN_POINT('Ctrl Pts',(0.125,-0.45,-0.379967103839267));
#12282=CARTESIAN_POINT('Ctrl Pts',(0.125,-0.465813100629203,-0.379967103839267));
#12283=CARTESIAN_POINT('Ctrl Pts',(0.121817958968287,-0.48260129709332,
-0.381057715344782));
#12284=CARTESIAN_POINT('Ctrl Pts',(0.109029967924066,-0.51336346023721,
-0.384911758361269));
#12285=CARTESIAN_POINT('Ctrl Pts',(0.0994291026068839,-0.527347592689753,
-0.38761064154154));
#12286=CARTESIAN_POINT('Ctrl Pts',(0.0773514949786257,-0.549425200318011,
-0.392612801026882));
#12287=CARTESIAN_POINT('Ctrl Pts',(0.0633657881355918,-0.559029081159106,
-0.395252954914593));
#12288=CARTESIAN_POINT('Ctrl Pts',(0.0325978607437828,-0.571819306519379,
-0.398970551469948));
#12289=CARTESIAN_POINT('Ctrl Pts',(0.0158075115832676,-0.575,-0.4));
#12290=CARTESIAN_POINT('Ctrl Pts',(-0.0158075115832676,-0.575,-0.4));
#12291=CARTESIAN_POINT('Ctrl Pts',(-0.0325978607437828,-0.571819306519379,
-0.398970551469948));
#12292=CARTESIAN_POINT('Ctrl Pts',(-0.0633657881355918,-0.559029081159106,
-0.395252954914593));
#12293=CARTESIAN_POINT('Ctrl Pts',(-0.0773514949786256,-0.549425200318011,
-0.392612801026882));
#12294=CARTESIAN_POINT('Ctrl Pts',(-0.0994291026068839,-0.527347592689753,
-0.38761064154154));
#12295=CARTESIAN_POINT('Ctrl Pts',(-0.109029967924066,-0.51336346023721,
-0.384911758361269));
#12296=CARTESIAN_POINT('Ctrl Pts',(-0.121817958968287,-0.48260129709332,
-0.381057715344782));
#12297=CARTESIAN_POINT('Ctrl Pts',(-0.125,-0.465813100629203,-0.379967103839267));
#12298=CARTESIAN_POINT('Ctrl Pts',(-0.125,-0.45,-0.379967103839267));
#12299=CARTESIAN_POINT('Ctrl Pts',(-0.125,-0.45,-0.379967103839267));
#12300=CARTESIAN_POINT('Ctrl Pts',(-0.125,-0.434186899370797,-0.379967103839267));
#12301=CARTESIAN_POINT('Ctrl Pts',(-0.121817958968287,-0.41739870290668,
-0.381057715344782));
#12302=CARTESIAN_POINT('Ctrl Pts',(-0.109029967924066,-0.38663653976279,
-0.384911758361269));
#12303=CARTESIAN_POINT('Ctrl Pts',(-0.0994291026068839,-0.372652407310247,
-0.38761064154154));
#12304=CARTESIAN_POINT('Ctrl Pts',(-0.0773514949786257,-0.350574799681989,
-0.392612801026882));
#12305=CARTESIAN_POINT('Ctrl Pts',(-0.0633657881355918,-0.340970918840894,
-0.395252954914593));
#12306=CARTESIAN_POINT('Ctrl Pts',(-0.0325978607437829,-0.328180693480621,
-0.398970551469948));
#12307=CARTESIAN_POINT('Ctrl Pts',(-0.0158075115832676,-0.325,-0.4));
#12308=CARTESIAN_POINT('Ctrl Pts',(0.0158075115832675,-0.325,-0.4));
#12309=CARTESIAN_POINT('Ctrl Pts',(0.0325978607437828,-0.328180693480621,
-0.398970551469948));
#12310=CARTESIAN_POINT('Ctrl Pts',(0.0633657881355917,-0.340970918840894,
-0.395252954914593));
#12311=CARTESIAN_POINT('Ctrl Pts',(0.0773514949786256,-0.350574799681989,
-0.392612801026882));
#12312=CARTESIAN_POINT('Ctrl Pts',(0.0994291026068839,-0.372652407310247,
-0.38761064154154));
#12313=CARTESIAN_POINT('Ctrl Pts',(0.109029967924066,-0.38663653976279,
-0.384911758361269));
#12314=CARTESIAN_POINT('Ctrl Pts',(0.121817958968287,-0.41739870290668,
-0.381057715344782));
#12315=CARTESIAN_POINT('Ctrl Pts',(0.125,-0.434186899370797,-0.379967103839267));
#12316=CARTESIAN_POINT('Ctrl Pts',(0.125,-0.45,-0.379967103839267));
#12317=CARTESIAN_POINT('Origin',(0.,-0.45,0.));
#12318=CARTESIAN_POINT('',(0.125,-0.45,0.379967103839267));
#12319=CARTESIAN_POINT('',(-0.125,-0.45,0.379967103839267));
#12320=CARTESIAN_POINT('Ctrl Pts',(0.125,-0.45,0.379967103839267));
#12321=CARTESIAN_POINT('Ctrl Pts',(0.125,-0.434186899370797,0.379967103839267));
#12322=CARTESIAN_POINT('Ctrl Pts',(0.121817958968287,-0.41739870290668,
0.381057715344782));
#12323=CARTESIAN_POINT('Ctrl Pts',(0.109029967924066,-0.38663653976279,
0.384911758361269));
#12324=CARTESIAN_POINT('Ctrl Pts',(0.0994291026068839,-0.372652407310247,
0.38761064154154));
#12325=CARTESIAN_POINT('Ctrl Pts',(0.0773514949786256,-0.350574799681989,
0.392612801026882));
#12326=CARTESIAN_POINT('Ctrl Pts',(0.0633657881355918,-0.340970918840894,
0.395252954914593));
#12327=CARTESIAN_POINT('Ctrl Pts',(0.0325978607437828,-0.328180693480621,
0.398970551469948));
#12328=CARTESIAN_POINT('Ctrl Pts',(0.0158075115832676,-0.325,0.4));
#12329=CARTESIAN_POINT('Ctrl Pts',(-0.0158075115832676,-0.325,0.4));
#12330=CARTESIAN_POINT('Ctrl Pts',(-0.0325978607437828,-0.328180693480621,
0.398970551469948));
#12331=CARTESIAN_POINT('Ctrl Pts',(-0.0633657881355918,-0.340970918840894,
0.395252954914593));
#12332=CARTESIAN_POINT('Ctrl Pts',(-0.0773514949786257,-0.350574799681989,
0.392612801026882));
#12333=CARTESIAN_POINT('Ctrl Pts',(-0.0994291026068839,-0.372652407310247,
0.38761064154154));
#12334=CARTESIAN_POINT('Ctrl Pts',(-0.109029967924066,-0.38663653976279,
0.384911758361269));
#12335=CARTESIAN_POINT('Ctrl Pts',(-0.121817958968287,-0.41739870290668,
0.381057715344782));
#12336=CARTESIAN_POINT('Ctrl Pts',(-0.125,-0.434186899370797,0.379967103839267));
#12337=CARTESIAN_POINT('Ctrl Pts',(-0.125,-0.45,0.379967103839267));
#12338=CARTESIAN_POINT('Ctrl Pts',(-0.125,-0.45,0.379967103839267));
#12339=CARTESIAN_POINT('Ctrl Pts',(-0.125,-0.465813100629203,0.379967103839267));
#12340=CARTESIAN_POINT('Ctrl Pts',(-0.121817958968287,-0.48260129709332,
0.381057715344782));
#12341=CARTESIAN_POINT('Ctrl Pts',(-0.109029967924066,-0.51336346023721,
0.384911758361269));
#12342=CARTESIAN_POINT('Ctrl Pts',(-0.0994291026068839,-0.527347592689753,
0.38761064154154));
#12343=CARTESIAN_POINT('Ctrl Pts',(-0.0773514949786256,-0.549425200318011,
0.392612801026882));
#12344=CARTESIAN_POINT('Ctrl Pts',(-0.0633657881355917,-0.559029081159106,
0.395252954914593));
#12345=CARTESIAN_POINT('Ctrl Pts',(-0.0325978607437828,-0.571819306519379,
0.398970551469948));
#12346=CARTESIAN_POINT('Ctrl Pts',(-0.0158075115832675,-0.575,0.4));
#12347=CARTESIAN_POINT('Ctrl Pts',(0.0158075115832676,-0.575,0.4));
#12348=CARTESIAN_POINT('Ctrl Pts',(0.0325978607437828,-0.571819306519379,
0.398970551469948));
#12349=CARTESIAN_POINT('Ctrl Pts',(0.0633657881355917,-0.559029081159106,
0.395252954914593));
#12350=CARTESIAN_POINT('Ctrl Pts',(0.0773514949786257,-0.549425200318011,
0.392612801026882));
#12351=CARTESIAN_POINT('Ctrl Pts',(0.0994291026068839,-0.527347592689753,
0.38761064154154));
#12352=CARTESIAN_POINT('Ctrl Pts',(0.109029967924066,-0.51336346023721,
0.384911758361269));
#12353=CARTESIAN_POINT('Ctrl Pts',(0.121817958968287,-0.48260129709332,
0.381057715344782));
#12354=CARTESIAN_POINT('Ctrl Pts',(0.125,-0.465813100629203,0.379967103839267));
#12355=CARTESIAN_POINT('Ctrl Pts',(0.125,-0.45,0.379967103839267));
#12356=CARTESIAN_POINT('',(-0.125,-0.45,0.));
#12357=CARTESIAN_POINT('Origin',(0.,0.,0.));
#12358=CARTESIAN_POINT('',(-0.4,-0.8,4.89858719658941E-17));
#12359=CARTESIAN_POINT('Origin',(0.,-0.8,0.));
#12360=CARTESIAN_POINT('',(-0.4,0.,4.89858719658941E-17));
#12361=CARTESIAN_POINT('',(-0.4,0.85,-4.89858719658941E-17));
#12362=CARTESIAN_POINT('',(-0.4,0.,4.89858719658941E-17));
#12363=CARTESIAN_POINT('Origin',(0.,0.85,0.));
#12364=CARTESIAN_POINT('Origin',(0.,-0.8,0.));
#12365=CARTESIAN_POINT('Origin',(0.,0.,0.));
#12366=CARTESIAN_POINT('',(-0.8,0.,9.79717439317883E-17));
#12367=CARTESIAN_POINT('Origin',(0.,0.,0.));
#12368=CARTESIAN_POINT('',(0.595438916863769,0.,0.137993139022126));
#12369=CARTESIAN_POINT('',(0.562830534889751,0.,0.238351419397483));
#12370=CARTESIAN_POINT('Origin',(0.562758945330873,0.,0.182851465569258));
#12371=CARTESIAN_POINT('',(0.523653836874034,0.,0.315240018494132));
#12372=CARTESIAN_POINT('Origin',(0.,0.,0.));
#12373=CARTESIAN_POINT('',(0.461629008549572,0.,0.40060987082025));
#12374=CARTESIAN_POINT('Origin',(0.478711351753049,0.,0.347804155687524));
#12375=CARTESIAN_POINT('',(0.40060987082025,0.,0.461629008549572));
#12376=CARTESIAN_POINT('Origin',(0.,0.,0.));
#12377=CARTESIAN_POINT('',(0.315240018494132,0.,0.523653836874034));
#12378=CARTESIAN_POINT('Origin',(0.347804155687523,0.,0.478711351753049));
#12379=CARTESIAN_POINT('',(0.238351419397483,0.,0.562830534889751));
#12380=CARTESIAN_POINT('Origin',(0.,0.,0.));
#12381=CARTESIAN_POINT('',(0.137993139022126,0.,0.595438916863769));
#12382=CARTESIAN_POINT('Origin',(0.182851465569258,0.,0.562758945330873));
#12383=CARTESIAN_POINT('',(0.0527614703521001,0.,0.608938287003997));
#12384=CARTESIAN_POINT('Origin',(0.,0.,0.));
#12385=CARTESIAN_POINT('',(-0.0527614703521003,0.,0.608938287003997));
#12386=CARTESIAN_POINT('Origin',(-1.08697158783324E-16,0.,0.591719772367581));
#12387=CARTESIAN_POINT('',(-0.137993139022126,0.,0.595438916863769));
#12388=CARTESIAN_POINT('Origin',(0.,0.,0.));
#12389=CARTESIAN_POINT('',(-0.238351419397483,0.,0.562830534889751));
#12390=CARTESIAN_POINT('Origin',(-0.182851465569258,0.,0.562758945330873));
#12391=CARTESIAN_POINT('',(-0.315240018494132,0.,0.523653836874034));
#12392=CARTESIAN_POINT('Origin',(0.,0.,0.));
#12393=CARTESIAN_POINT('',(-0.40060987082025,0.,0.461629008549572));
#12394=CARTESIAN_POINT('Origin',(-0.347804155687524,0.,0.478711351753049));
#12395=CARTESIAN_POINT('',(-0.461629008549572,0.,0.40060987082025));
#12396=CARTESIAN_POINT('Origin',(0.,0.,0.));
#12397=CARTESIAN_POINT('',(-0.523653836874034,0.,0.315240018494132));
#12398=CARTESIAN_POINT('Origin',(-0.478711351753049,0.,0.347804155687524));
#12399=CARTESIAN_POINT('',(-0.562830534889751,0.,0.238351419397483));
#12400=CARTESIAN_POINT('Origin',(0.,0.,0.));
#12401=CARTESIAN_POINT('',(-0.595438916863769,0.,0.137993139022126));
#12402=CARTESIAN_POINT('Origin',(-0.562758945330873,0.,0.182851465569258));
#12403=CARTESIAN_POINT('',(-0.608938287003997,0.,0.0527614703521002));
#12404=CARTESIAN_POINT('Origin',(0.,0.,0.));
#12405=CARTESIAN_POINT('',(-0.608938287003997,0.,-0.0527614703521003));
#12406=CARTESIAN_POINT('Origin',(-0.591719772367581,0.,-7.24647725222159E-17));
#12407=CARTESIAN_POINT('',(-0.595438916863769,0.,-0.137993139022126));
#12408=CARTESIAN_POINT('Origin',(0.,0.,0.));
#12409=CARTESIAN_POINT('',(-0.562830534889751,0.,-0.238351419397483));
#12410=CARTESIAN_POINT('Origin',(-0.562758945330873,0.,-0.182851465569258));
#12411=CARTESIAN_POINT('',(-0.523653836874034,0.,-0.315240018494132));
#12412=CARTESIAN_POINT('Origin',(0.,0.,0.));
#12413=CARTESIAN_POINT('',(-0.461629008549572,0.,-0.40060987082025));
#12414=CARTESIAN_POINT('Origin',(-0.478711351753049,0.,-0.347804155687524));
#12415=CARTESIAN_POINT('',(-0.40060987082025,0.,-0.461629008549572));
#12416=CARTESIAN_POINT('Origin',(0.,0.,0.));
#12417=CARTESIAN_POINT('',(-0.315240018494132,0.,-0.523653836874034));
#12418=CARTESIAN_POINT('Origin',(-0.347804155687524,0.,-0.478711351753049));
#12419=CARTESIAN_POINT('',(-0.238351419397483,0.,-0.562830534889751));
#12420=CARTESIAN_POINT('Origin',(0.,0.,0.));
#12421=CARTESIAN_POINT('',(-0.137993139022126,0.,-0.595438916863769));
#12422=CARTESIAN_POINT('Origin',(-0.182851465569258,0.,-0.562758945330873));
#12423=CARTESIAN_POINT('',(-0.0527614703521002,0.,-0.608938287003997));
#12424=CARTESIAN_POINT('Origin',(0.,0.,0.));
#12425=CARTESIAN_POINT('',(0.0527614703521003,0.,-0.608938287003997));
#12426=CARTESIAN_POINT('Origin',(3.6232386261108E-17,0.,-0.591719772367581));
#12427=CARTESIAN_POINT('',(0.137993139022126,0.,-0.595438916863769));
#12428=CARTESIAN_POINT('Origin',(0.,0.,0.));
#12429=CARTESIAN_POINT('',(0.238351419397483,0.,-0.562830534889751));
#12430=CARTESIAN_POINT('Origin',(0.182851465569258,0.,-0.562758945330873));
#12431=CARTESIAN_POINT('',(0.315240018494132,0.,-0.523653836874034));
#12432=CARTESIAN_POINT('Origin',(0.,0.,0.));
#12433=CARTESIAN_POINT('',(0.40060987082025,0.,-0.461629008549572));
#12434=CARTESIAN_POINT('Origin',(0.347804155687524,0.,-0.478711351753049));
#12435=CARTESIAN_POINT('',(0.461629008549572,0.,-0.40060987082025));
#12436=CARTESIAN_POINT('Origin',(0.,0.,0.));
#12437=CARTESIAN_POINT('',(0.523653836874034,0.,-0.315240018494132));
#12438=CARTESIAN_POINT('Origin',(0.478711351753049,0.,-0.347804155687524));
#12439=CARTESIAN_POINT('',(0.562830534889751,0.,-0.238351419397483));
#12440=CARTESIAN_POINT('Origin',(0.,0.,0.));
#12441=CARTESIAN_POINT('',(0.595438916863769,0.,-0.137993139022126));
#12442=CARTESIAN_POINT('Origin',(0.562758945330873,0.,-0.182851465569258));
#12443=CARTESIAN_POINT('',(0.608938287003997,0.,-0.0527614703521001));
#12444=CARTESIAN_POINT('Origin',(0.,0.,0.));
#12445=CARTESIAN_POINT('',(0.608938287003997,0.,0.0527614703521001));
#12446=CARTESIAN_POINT('Origin',(0.591719772367581,0.,0.));
#12447=CARTESIAN_POINT('Origin',(0.,0.,0.));
#12448=CARTESIAN_POINT('Origin',(0.,0.,0.));
#12449=CARTESIAN_POINT('',(-0.8,-0.1,9.79717439317883E-17));
#12450=CARTESIAN_POINT('Origin',(0.,-0.1,0.));
#12451=CARTESIAN_POINT('',(-0.8,0.,-9.79717439317883E-17));
#12452=CARTESIAN_POINT('Origin',(0.,-0.1,0.));
#12453=CARTESIAN_POINT('Origin',(0.,0.75,0.));
#12454=CARTESIAN_POINT('',(-0.8,0.75,9.79717439317883E-17));
#12455=CARTESIAN_POINT('Origin',(0.,0.75,0.));
#12456=CARTESIAN_POINT('',(0.562830534889751,0.75,0.238351419397483));
#12457=CARTESIAN_POINT('',(0.595438916863769,0.75,0.137993139022126));
#12458=CARTESIAN_POINT('Origin',(0.562758945330873,0.75,0.182851465569258));
#12459=CARTESIAN_POINT('',(0.608938287003997,0.75,0.0527614703521002));
#12460=CARTESIAN_POINT('Origin',(0.,0.75,0.));
#12461=CARTESIAN_POINT('',(0.608938287003997,0.75,-0.0527614703521002));
#12462=CARTESIAN_POINT('Origin',(0.591719772367581,0.75,0.));
#12463=CARTESIAN_POINT('',(0.595438916863769,0.75,-0.137993139022126));
#12464=CARTESIAN_POINT('Origin',(0.,0.75,0.));
#12465=CARTESIAN_POINT('',(0.562830534889751,0.75,-0.238351419397483));
#12466=CARTESIAN_POINT('Origin',(0.562758945330873,0.75,-0.182851465569258));
#12467=CARTESIAN_POINT('',(0.523653836874034,0.75,-0.315240018494132));
#12468=CARTESIAN_POINT('Origin',(0.,0.75,0.));
#12469=CARTESIAN_POINT('',(0.461629008549572,0.75,-0.40060987082025));
#12470=CARTESIAN_POINT('Origin',(0.478711351753049,0.75,-0.347804155687524));
#12471=CARTESIAN_POINT('',(0.40060987082025,0.75,-0.461629008549572));
#12472=CARTESIAN_POINT('Origin',(0.,0.75,0.));
#12473=CARTESIAN_POINT('',(0.315240018494132,0.75,-0.523653836874034));
#12474=CARTESIAN_POINT('Origin',(0.347804155687524,0.75,-0.478711351753049));
#12475=CARTESIAN_POINT('',(0.238351419397483,0.75,-0.562830534889751));
#12476=CARTESIAN_POINT('Origin',(0.,0.75,0.));
#12477=CARTESIAN_POINT('',(0.137993139022126,0.75,-0.595438916863769));
#12478=CARTESIAN_POINT('Origin',(0.182851465569258,0.75,-0.562758945330873));
#12479=CARTESIAN_POINT('',(0.0527614703521003,0.75,-0.608938287003997));
#12480=CARTESIAN_POINT('Origin',(0.,0.75,0.));
#12481=CARTESIAN_POINT('',(-0.0527614703521002,0.75,-0.608938287003997));
#12482=CARTESIAN_POINT('Origin',(3.6232386261108E-17,0.75,-0.591719772367581));
#12483=CARTESIAN_POINT('',(-0.137993139022126,0.75,-0.595438916863769));
#12484=CARTESIAN_POINT('Origin',(0.,0.75,0.));
#12485=CARTESIAN_POINT('',(-0.238351419397483,0.75,-0.562830534889751));
#12486=CARTESIAN_POINT('Origin',(-0.182851465569258,0.75,-0.562758945330873));
#12487=CARTESIAN_POINT('',(-0.315240018494132,0.75,-0.523653836874034));
#12488=CARTESIAN_POINT('Origin',(0.,0.75,0.));
#12489=CARTESIAN_POINT('',(-0.40060987082025,0.75,-0.461629008549572));
#12490=CARTESIAN_POINT('Origin',(-0.347804155687524,0.75,-0.478711351753049));
#12491=CARTESIAN_POINT('',(-0.461629008549572,0.75,-0.40060987082025));
#12492=CARTESIAN_POINT('Origin',(0.,0.75,0.));
#12493=CARTESIAN_POINT('',(-0.523653836874034,0.75,-0.315240018494132));
#12494=CARTESIAN_POINT('Origin',(-0.478711351753049,0.75,-0.347804155687524));
#12495=CARTESIAN_POINT('',(-0.562830534889751,0.75,-0.238351419397483));
#12496=CARTESIAN_POINT('Origin',(0.,0.75,0.));
#12497=CARTESIAN_POINT('',(-0.595438916863769,0.75,-0.137993139022126));
#12498=CARTESIAN_POINT('Origin',(-0.562758945330873,0.75,-0.182851465569258));
#12499=CARTESIAN_POINT('',(-0.608938287003997,0.75,-0.0527614703521003));
#12500=CARTESIAN_POINT('Origin',(0.,0.75,0.));
#12501=CARTESIAN_POINT('',(-0.608938287003997,0.75,0.0527614703521002));
#12502=CARTESIAN_POINT('Origin',(-0.591719772367581,0.75,-7.24647725222159E-17));
#12503=CARTESIAN_POINT('',(-0.595438916863769,0.75,0.137993139022126));
#12504=CARTESIAN_POINT('Origin',(0.,0.75,0.));
#12505=CARTESIAN_POINT('',(-0.562830534889751,0.75,0.238351419397483));
#12506=CARTESIAN_POINT('Origin',(-0.562758945330873,0.75,0.182851465569258));
#12507=CARTESIAN_POINT('',(-0.523653836874034,0.75,0.315240018494132));
#12508=CARTESIAN_POINT('Origin',(0.,0.75,0.));
#12509=CARTESIAN_POINT('',(-0.461629008549572,0.75,0.40060987082025));
#12510=CARTESIAN_POINT('Origin',(-0.478711351753049,0.75,0.347804155687524));
#12511=CARTESIAN_POINT('',(-0.40060987082025,0.75,0.461629008549572));
#12512=CARTESIAN_POINT('Origin',(0.,0.75,0.));
#12513=CARTESIAN_POINT('',(-0.315240018494132,0.75,0.523653836874034));
#12514=CARTESIAN_POINT('Origin',(-0.347804155687524,0.75,0.478711351753049));
#12515=CARTESIAN_POINT('',(-0.238351419397483,0.75,0.562830534889751));
#12516=CARTESIAN_POINT('Origin',(0.,0.75,0.));
#12517=CARTESIAN_POINT('',(-0.137993139022126,0.75,0.595438916863769));
#12518=CARTESIAN_POINT('Origin',(-0.182851465569258,0.75,0.562758945330873));
#12519=CARTESIAN_POINT('',(-0.0527614703521003,0.75,0.608938287003997));
#12520=CARTESIAN_POINT('Origin',(0.,0.75,0.));
#12521=CARTESIAN_POINT('',(0.0527614703521001,0.75,0.608938287003997));
#12522=CARTESIAN_POINT('Origin',(-1.08697158783324E-16,0.75,0.591719772367581));
#12523=CARTESIAN_POINT('',(0.137993139022126,0.75,0.595438916863769));
#12524=CARTESIAN_POINT('Origin',(0.,0.75,0.));
#12525=CARTESIAN_POINT('',(0.238351419397483,0.75,0.562830534889751));
#12526=CARTESIAN_POINT('Origin',(0.182851465569258,0.75,0.562758945330873));
#12527=CARTESIAN_POINT('',(0.315240018494132,0.75,0.523653836874034));
#12528=CARTESIAN_POINT('Origin',(0.,0.75,0.));
#12529=CARTESIAN_POINT('',(0.40060987082025,0.75,0.461629008549572));
#12530=CARTESIAN_POINT('Origin',(0.347804155687523,0.75,0.478711351753049));
#12531=CARTESIAN_POINT('',(0.461629008549572,0.75,0.40060987082025));
#12532=CARTESIAN_POINT('Origin',(0.,0.75,0.));
#12533=CARTESIAN_POINT('',(0.523653836874034,0.75,0.315240018494132));
#12534=CARTESIAN_POINT('Origin',(0.478711351753049,0.75,0.347804155687524));
#12535=CARTESIAN_POINT('Origin',(0.,0.75,0.));
#12536=CARTESIAN_POINT('Origin',(0.,0.75,0.));
#12537=CARTESIAN_POINT('',(-0.8,0.85,9.79717439317883E-17));
#12538=CARTESIAN_POINT('Origin',(0.,0.85,0.));
#12539=CARTESIAN_POINT('',(-0.8,0.75,9.79717439317883E-17));
#12540=CARTESIAN_POINT('Origin',(0.,0.85,0.));
#12541=CARTESIAN_POINT('Origin',(0.562758945330873,0.,0.182851465569258));
#12542=CARTESIAN_POINT('',(0.595438916863769,0.,0.137993139022126));
#12543=CARTESIAN_POINT('',(0.562830534889751,0.,0.238351419397483));
#12544=CARTESIAN_POINT('Origin',(0.,0.,0.));
#12545=CARTESIAN_POINT('',(0.523653836874034,0.,0.315240018494132));
#12546=CARTESIAN_POINT('Origin',(0.478711351753049,0.,0.347804155687524));
#12547=CARTESIAN_POINT('',(0.461629008549572,0.,0.40060987082025));
#12548=CARTESIAN_POINT('Origin',(0.,0.,0.));
#12549=CARTESIAN_POINT('',(0.40060987082025,0.,0.461629008549572));
#12550=CARTESIAN_POINT('Origin',(0.347804155687523,0.,0.478711351753049));
#12551=CARTESIAN_POINT('',(0.315240018494132,0.,0.523653836874034));
#12552=CARTESIAN_POINT('Origin',(0.,0.,0.));
#12553=CARTESIAN_POINT('',(0.238351419397483,0.,0.562830534889751));
#12554=CARTESIAN_POINT('Origin',(0.182851465569258,0.,0.562758945330873));
#12555=CARTESIAN_POINT('',(0.137993139022126,0.,0.595438916863769));
#12556=CARTESIAN_POINT('Origin',(0.,0.,0.));
#12557=CARTESIAN_POINT('',(0.0527614703521,0.,0.608938287003997));
#12558=CARTESIAN_POINT('Origin',(-1.08697158783324E-16,0.,0.591719772367581));
#12559=CARTESIAN_POINT('',(-0.0527614703521002,0.,0.608938287003997));
#12560=CARTESIAN_POINT('Origin',(0.,0.,0.));
#12561=CARTESIAN_POINT('',(-0.137993139022126,0.,0.595438916863769));
#12562=CARTESIAN_POINT('Origin',(-0.182851465569258,0.,0.562758945330873));
#12563=CARTESIAN_POINT('',(-0.238351419397483,0.,0.562830534889751));
#12564=CARTESIAN_POINT('Origin',(0.,0.,0.));
#12565=CARTESIAN_POINT('',(-0.315240018494132,0.,0.523653836874034));
#12566=CARTESIAN_POINT('Origin',(-0.347804155687524,0.,0.478711351753049));
#12567=CARTESIAN_POINT('',(-0.40060987082025,0.,0.461629008549572));
#12568=CARTESIAN_POINT('Origin',(0.,0.,0.));
#12569=CARTESIAN_POINT('',(-0.461629008549572,0.,0.40060987082025));
#12570=CARTESIAN_POINT('Origin',(-0.478711351753049,0.,0.347804155687524));
#12571=CARTESIAN_POINT('',(-0.523653836874034,0.,0.315240018494132));
#12572=CARTESIAN_POINT('Origin',(0.,0.,0.));
#12573=CARTESIAN_POINT('',(-0.562830534889751,0.,0.238351419397483));
#12574=CARTESIAN_POINT('Origin',(-0.562758945330873,0.,0.182851465569258));
#12575=CARTESIAN_POINT('',(-0.595438916863769,0.,0.137993139022126));
#12576=CARTESIAN_POINT('Origin',(0.,0.,0.));
#12577=CARTESIAN_POINT('',(-0.608938287003997,0.,0.0527614703521));
#12578=CARTESIAN_POINT('Origin',(-0.591719772367581,0.,-7.24647725222159E-17));
#12579=CARTESIAN_POINT('',(-0.608938287003997,0.,-0.0527614703521002));
#12580=CARTESIAN_POINT('Origin',(0.,0.,0.));
#12581=CARTESIAN_POINT('',(-0.595438916863769,0.,-0.137993139022126));
#12582=CARTESIAN_POINT('Origin',(-0.562758945330873,0.,-0.182851465569258));
#12583=CARTESIAN_POINT('',(-0.562830534889751,0.,-0.238351419397483));
#12584=CARTESIAN_POINT('Origin',(0.,0.,0.));
#12585=CARTESIAN_POINT('',(-0.523653836874034,0.,-0.315240018494132));
#12586=CARTESIAN_POINT('Origin',(-0.478711351753049,0.,-0.347804155687524));
#12587=CARTESIAN_POINT('',(-0.461629008549572,0.,-0.40060987082025));
#12588=CARTESIAN_POINT('Origin',(0.,0.,0.));
#12589=CARTESIAN_POINT('',(-0.40060987082025,0.,-0.461629008549572));
#12590=CARTESIAN_POINT('Origin',(-0.347804155687524,0.,-0.478711351753049));
#12591=CARTESIAN_POINT('',(-0.315240018494132,0.,-0.523653836874034));
#12592=CARTESIAN_POINT('Origin',(0.,0.,0.));
#12593=CARTESIAN_POINT('',(-0.238351419397483,0.,-0.562830534889751));
#12594=CARTESIAN_POINT('Origin',(-0.182851465569258,0.,-0.562758945330873));
#12595=CARTESIAN_POINT('',(-0.137993139022126,0.,-0.595438916863769));
#12596=CARTESIAN_POINT('Origin',(0.,0.,0.));
#12597=CARTESIAN_POINT('',(-0.0527614703521,0.,-0.608938287003997));
#12598=CARTESIAN_POINT('Origin',(3.6232386261108E-17,0.,-0.591719772367581));
#12599=CARTESIAN_POINT('',(0.0527614703521001,0.,-0.608938287003997));
#12600=CARTESIAN_POINT('Origin',(0.,0.,0.));
#12601=CARTESIAN_POINT('',(0.137993139022126,0.,-0.595438916863769));
#12602=CARTESIAN_POINT('Origin',(0.182851465569258,0.,-0.562758945330873));
#12603=CARTESIAN_POINT('',(0.238351419397483,0.,-0.562830534889751));
#12604=CARTESIAN_POINT('Origin',(0.,0.,0.));
#12605=CARTESIAN_POINT('',(0.315240018494132,0.,-0.523653836874034));
#12606=CARTESIAN_POINT('Origin',(0.347804155687524,0.,-0.478711351753049));
#12607=CARTESIAN_POINT('',(0.40060987082025,0.,-0.461629008549572));
#12608=CARTESIAN_POINT('Origin',(0.,0.,0.));
#12609=CARTESIAN_POINT('',(0.461629008549572,0.,-0.40060987082025));
#12610=CARTESIAN_POINT('Origin',(0.478711351753049,0.,-0.347804155687524));
#12611=CARTESIAN_POINT('',(0.523653836874034,0.,-0.315240018494132));
#12612=CARTESIAN_POINT('Origin',(0.,0.,0.));
#12613=CARTESIAN_POINT('',(0.562830534889751,0.,-0.238351419397483));
#12614=CARTESIAN_POINT('Origin',(0.562758945330873,0.,-0.182851465569258));
#12615=CARTESIAN_POINT('',(0.595438916863769,0.,-0.137993139022126));
#12616=CARTESIAN_POINT('Origin',(0.,0.,0.));
#12617=CARTESIAN_POINT('',(0.608938287003997,0.,0.0527614703521001));
#12618=CARTESIAN_POINT('Origin',(0.591719772367581,0.,0.));
#12619=CARTESIAN_POINT('',(0.608938287003997,0.,-0.0527614703521001));
#12620=CARTESIAN_POINT('Origin',(0.,0.,0.));
#12621=CARTESIAN_POINT('',(0.,0.,0.));
#12622=CARTESIAN_POINT('Origin',(0.0866025403784439,-0.4,-0.15));
#12623=CARTESIAN_POINT('',(0.173205080756888,-0.4,0.));
#12624=CARTESIAN_POINT('',(0.0866025403784439,-0.4,-0.15));
#12625=CARTESIAN_POINT('',(0.173205080756888,-0.4,0.));
#12626=CARTESIAN_POINT('',(0.0866025403784439,-0.64,-0.15));
#12627=CARTESIAN_POINT('',(0.0866025403784439,-0.4,-0.15));
#12628=CARTESIAN_POINT('',(0.173205080756888,-0.64,0.));
#12629=CARTESIAN_POINT('',(0.173205080756888,-0.64,0.));
#12630=CARTESIAN_POINT('',(0.173205080756888,-0.4,0.));
#12631=CARTESIAN_POINT('Origin',(-0.0866025403784438,-0.4,-0.15));
#12632=CARTESIAN_POINT('',(-0.0866025403784438,-0.4,-0.15));
#12633=CARTESIAN_POINT('',(0.0866025403784439,-0.4,-0.15));
#12634=CARTESIAN_POINT('',(-0.0866025403784438,-0.64,-0.15));
#12635=CARTESIAN_POINT('',(-0.0866025403784438,-0.4,-0.15));
#12636=CARTESIAN_POINT('',(0.0866025403784439,-0.64,-0.15));
#12637=CARTESIAN_POINT('Origin',(-0.173205080756888,-0.4,-2.77555756156289E-17));
#12638=CARTESIAN_POINT('',(-0.173205080756888,-0.4,-2.12115047744981E-17));
#12639=CARTESIAN_POINT('',(-0.0866025403784438,-0.4,-0.15));
#12640=CARTESIAN_POINT('',(-0.173205080756888,-0.64,-2.77555756156289E-17));
#12641=CARTESIAN_POINT('',(-0.173205080756888,-0.4,-2.12115047744981E-17));
#12642=CARTESIAN_POINT('',(-0.0866025403784438,-0.64,-0.15));
#12643=CARTESIAN_POINT('Origin',(-0.0866025403784439,-0.4,0.15));
#12644=CARTESIAN_POINT('',(-0.0866025403784439,-0.4,0.15));
#12645=CARTESIAN_POINT('',(-0.173205080756888,-0.4,-2.12115047744981E-17));
#12646=CARTESIAN_POINT('',(-0.0866025403784439,-0.64,0.15));
#12647=CARTESIAN_POINT('',(-0.0866025403784439,-0.4,0.15));
#12648=CARTESIAN_POINT('',(-0.173205080756888,-0.64,-2.12115047744981E-17));
#12649=CARTESIAN_POINT('Origin',(0.0866025403784439,-0.4,0.15));
#12650=CARTESIAN_POINT('',(0.0866025403784439,-0.4,0.15));
#12651=CARTESIAN_POINT('',(-0.0866025403784439,-0.4,0.15));
#12652=CARTESIAN_POINT('',(0.0866025403784439,-0.64,0.15));
#12653=CARTESIAN_POINT('',(0.0866025403784439,-0.4,0.15));
#12654=CARTESIAN_POINT('',(-0.0866025403784439,-0.64,0.15));
#12655=CARTESIAN_POINT('Origin',(0.173205080756888,-0.4,0.));
#12656=CARTESIAN_POINT('',(0.0866025403784439,-0.4,0.15));
#12657=CARTESIAN_POINT('',(0.0866025403784439,-0.64,0.15));
#12658=CARTESIAN_POINT('Origin',(0.,-0.4,-2.77555756156289E-17));
#12659=CARTESIAN_POINT('Origin',(0.,-0.64,-2.77555756156289E-17));
#12660=CARTESIAN_POINT('Origin',(0.,-1.,0.));
#12661=CARTESIAN_POINT('',(-0.1954,-1.,2.39295984553393E-17));
#12662=CARTESIAN_POINT('Origin',(0.,-1.,0.));
#12663=CARTESIAN_POINT('Origin',(0.3,0.4,0.));
#12664=CARTESIAN_POINT('',(-0.3,0.4,-3.67394039744206E-17));
#12665=CARTESIAN_POINT('Origin',(0.,0.4,0.));
#12666=CARTESIAN_POINT('Origin',(0.,0.375,0.));
#12667=CARTESIAN_POINT('',(-0.35,0.35,-4.28626379701573E-17));
#12668=CARTESIAN_POINT('Origin',(0.,0.35,0.));
#12669=CARTESIAN_POINT('',(-0.325,0.375,-3.9801020972289E-17));
#12670=CARTESIAN_POINT('Origin',(0.,0.19,0.));
#12671=CARTESIAN_POINT('',(-0.35,0.03,-4.28626379701574E-17));
#12672=CARTESIAN_POINT('Origin',(0.,0.03,0.));
#12673=CARTESIAN_POINT('',(-0.35,0.19,-4.28626379701574E-17));
#12674=CARTESIAN_POINT('Origin',(0.,0.0149999999999999,0.));
#12675=CARTESIAN_POINT('',(-0.32,-3.29597460435593E-17,-3.91886975727153E-17));
#12676=CARTESIAN_POINT('Origin',(0.,0.,0.));
#12677=CARTESIAN_POINT('',(-0.335,0.0149999999999999,-4.10256677714363E-17));
#12678=CARTESIAN_POINT('Origin',(0.22,0.,0.));
#12679=CARTESIAN_POINT('',(-0.22,-6.93889390390723E-18,-2.69422295812418E-17));
#12680=CARTESIAN_POINT('Origin',(0.,0.,0.));
#12681=CARTESIAN_POINT('Origin',(0.,-0.02,0.));
#12682=CARTESIAN_POINT('',(-0.1954,-0.0492,2.39295984553393E-17));
#12683=CARTESIAN_POINT('Origin',(0.,-0.0492,0.));
#12684=CARTESIAN_POINT('',(-0.21,-0.02,-2.57175827820944E-17));
#12685=CARTESIAN_POINT('Origin',(0.,-0.8,0.));
#12686=CARTESIAN_POINT('',(-0.1954,-0.8,-2.39295984553393E-17));
#12687=CARTESIAN_POINT('',(0.,0.,0.));
#12688=CARTESIAN_POINT('',(0.,0.,0.));
#12689=CARTESIAN_POINT('',(0.,0.,0.));
#12690=CARTESIAN_POINT('',(0.,0.,0.));
#12691=CARTESIAN_POINT('',(0.,0.,0.));
#12692=CARTESIAN_POINT('',(0.,0.,0.));
#12693=CARTESIAN_POINT('',(0.,0.,0.));
#12694=CARTESIAN_POINT('',(9.9,0.,4.65));
#12695=CARTESIAN_POINT('',(9.,0.,8.));
#12696=CARTESIAN_POINT('',(9.,0.,9.2));
#12697=CARTESIAN_POINT('',(0.,0.,0.));
#12698=CARTESIAN_POINT('',(0.,0.,0.));
#12699=CARTESIAN_POINT('',(0.,0.,0.));
#12700=UNCERTAINTY_MEASURE_WITH_UNIT(LENGTH_MEASURE(0.001),#12780,
'DISTANCE_ACCURACY_VALUE',
'Maximum model space distance between geometric entities at asserted c
onnectivities');
#12701=UNCERTAINTY_MEASURE_WITH_UNIT(LENGTH_MEASURE(0.001),#12780,
'DISTANCE_ACCURACY_VALUE',
'Maximum model space distance between geometric entities at asserted c
onnectivities');
#12702=UNCERTAINTY_MEASURE_WITH_UNIT(LENGTH_MEASURE(0.001),#12780,
'DISTANCE_ACCURACY_VALUE',
'Maximum model space distance between geometric entities at asserted c
onnectivities');
#12703=UNCERTAINTY_MEASURE_WITH_UNIT(LENGTH_MEASURE(0.001),#12780,
'DISTANCE_ACCURACY_VALUE',
'Maximum model space distance between geometric entities at asserted c
onnectivities');
#12704=UNCERTAINTY_MEASURE_WITH_UNIT(LENGTH_MEASURE(0.001),#12780,
'DISTANCE_ACCURACY_VALUE',
'Maximum model space distance between geometric entities at asserted c
onnectivities');
#12705=UNCERTAINTY_MEASURE_WITH_UNIT(LENGTH_MEASURE(0.001),#12780,
'DISTANCE_ACCURACY_VALUE',
'Maximum model space distance between geometric entities at asserted c
onnectivities');
#12706=UNCERTAINTY_MEASURE_WITH_UNIT(LENGTH_MEASURE(0.001),#12780,
'DISTANCE_ACCURACY_VALUE',
'Maximum model space distance between geometric entities at asserted c
onnectivities');
#12707=UNCERTAINTY_MEASURE_WITH_UNIT(LENGTH_MEASURE(0.001),#12780,
'DISTANCE_ACCURACY_VALUE',
'Maximum model space distance between geometric entities at asserted c
onnectivities');
#12708=UNCERTAINTY_MEASURE_WITH_UNIT(LENGTH_MEASURE(0.001),#12780,
'DISTANCE_ACCURACY_VALUE',
'Maximum model space distance between geometric entities at asserted c
onnectivities');
#12709=UNCERTAINTY_MEASURE_WITH_UNIT(LENGTH_MEASURE(0.001),#12780,
'DISTANCE_ACCURACY_VALUE',
'Maximum model space distance between geometric entities at asserted c
onnectivities');
#12710=UNCERTAINTY_MEASURE_WITH_UNIT(LENGTH_MEASURE(0.001),#12780,
'DISTANCE_ACCURACY_VALUE',
'Maximum model space distance between geometric entities at asserted c
onnectivities');
#12711=UNCERTAINTY_MEASURE_WITH_UNIT(LENGTH_MEASURE(0.001),#12780,
'DISTANCE_ACCURACY_VALUE',
'Maximum model space distance between geometric entities at asserted c
onnectivities');
#12712=UNCERTAINTY_MEASURE_WITH_UNIT(LENGTH_MEASURE(0.001),#12780,
'DISTANCE_ACCURACY_VALUE',
'Maximum model space distance between geometric entities at asserted c
onnectivities');
#12713=UNCERTAINTY_MEASURE_WITH_UNIT(LENGTH_MEASURE(0.001),#12780,
'DISTANCE_ACCURACY_VALUE',
'Maximum model space distance between geometric entities at asserted c
onnectivities');
#12714=UNCERTAINTY_MEASURE_WITH_UNIT(LENGTH_MEASURE(0.001),#12780,
'DISTANCE_ACCURACY_VALUE',
'Maximum model space distance between geometric entities at asserted c
onnectivities');
#12715=UNCERTAINTY_MEASURE_WITH_UNIT(LENGTH_MEASURE(0.001),#12780,
'DISTANCE_ACCURACY_VALUE',
'Maximum model space distance between geometric entities at asserted c
onnectivities');
#12716=UNCERTAINTY_MEASURE_WITH_UNIT(LENGTH_MEASURE(0.001),#12780,
'DISTANCE_ACCURACY_VALUE',
'Maximum model space distance between geometric entities at asserted c
onnectivities');
#12717=UNCERTAINTY_MEASURE_WITH_UNIT(LENGTH_MEASURE(0.001),#12780,
'DISTANCE_ACCURACY_VALUE',
'Maximum model space distance between geometric entities at asserted c
onnectivities');
#12718=UNCERTAINTY_MEASURE_WITH_UNIT(LENGTH_MEASURE(0.001),#12780,
'DISTANCE_ACCURACY_VALUE',
'Maximum model space distance between geometric entities at asserted c
onnectivities');
#12719=UNCERTAINTY_MEASURE_WITH_UNIT(LENGTH_MEASURE(0.001),#12780,
'DISTANCE_ACCURACY_VALUE',
'Maximum model space distance between geometric entities at asserted c
onnectivities');
#12720=UNCERTAINTY_MEASURE_WITH_UNIT(LENGTH_MEASURE(0.001),#12780,
'DISTANCE_ACCURACY_VALUE',
'Maximum model space distance between geometric entities at asserted c
onnectivities');
#12721=UNCERTAINTY_MEASURE_WITH_UNIT(LENGTH_MEASURE(0.001),#12780,
'DISTANCE_ACCURACY_VALUE',
'Maximum model space distance between geometric entities at asserted c
onnectivities');
#12722=UNCERTAINTY_MEASURE_WITH_UNIT(LENGTH_MEASURE(0.001),#12780,
'DISTANCE_ACCURACY_VALUE',
'Maximum model space distance between geometric entities at asserted c
onnectivities');
#12723=UNCERTAINTY_MEASURE_WITH_UNIT(LENGTH_MEASURE(0.001),#12780,
'DISTANCE_ACCURACY_VALUE',
'Maximum model space distance between geometric entities at asserted c
onnectivities');
#12724=UNCERTAINTY_MEASURE_WITH_UNIT(LENGTH_MEASURE(0.001),#12780,
'DISTANCE_ACCURACY_VALUE',
'Maximum model space distance between geometric entities at asserted c
onnectivities');
#12725=UNCERTAINTY_MEASURE_WITH_UNIT(LENGTH_MEASURE(0.001),#12780,
'DISTANCE_ACCURACY_VALUE',
'Maximum model space distance between geometric entities at asserted c
onnectivities');
#12726=UNCERTAINTY_MEASURE_WITH_UNIT(LENGTH_MEASURE(0.001),#12780,
'DISTANCE_ACCURACY_VALUE',
'Maximum model space distance between geometric entities at asserted c
onnectivities');
#12727=UNCERTAINTY_MEASURE_WITH_UNIT(LENGTH_MEASURE(0.001),#12780,
'DISTANCE_ACCURACY_VALUE',
'Maximum model space distance between geometric entities at asserted c
onnectivities');
#12728=UNCERTAINTY_MEASURE_WITH_UNIT(LENGTH_MEASURE(0.001),#12780,
'DISTANCE_ACCURACY_VALUE',
'Maximum model space distance between geometric entities at asserted c
onnectivities');
#12729=UNCERTAINTY_MEASURE_WITH_UNIT(LENGTH_MEASURE(0.001),#12780,
'DISTANCE_ACCURACY_VALUE',
'Maximum model space distance between geometric entities at asserted c
onnectivities');
#12730=UNCERTAINTY_MEASURE_WITH_UNIT(LENGTH_MEASURE(0.001),#12780,
'DISTANCE_ACCURACY_VALUE',
'Maximum model space distance between geometric entities at asserted c
onnectivities');
#12731=UNCERTAINTY_MEASURE_WITH_UNIT(LENGTH_MEASURE(0.001),#12780,
'DISTANCE_ACCURACY_VALUE',
'Maximum model space distance between geometric entities at asserted c
onnectivities');
#12732=UNCERTAINTY_MEASURE_WITH_UNIT(LENGTH_MEASURE(0.001),#12780,
'DISTANCE_ACCURACY_VALUE',
'Maximum model space distance between geometric entities at asserted c
onnectivities');
#12733=UNCERTAINTY_MEASURE_WITH_UNIT(LENGTH_MEASURE(0.001),#12780,
'DISTANCE_ACCURACY_VALUE',
'Maximum model space distance between geometric entities at asserted c
onnectivities');
#12734=UNCERTAINTY_MEASURE_WITH_UNIT(LENGTH_MEASURE(0.001),#12780,
'DISTANCE_ACCURACY_VALUE',
'Maximum model space distance between geometric entities at asserted c
onnectivities');
#12735=UNCERTAINTY_MEASURE_WITH_UNIT(LENGTH_MEASURE(0.001),#12780,
'DISTANCE_ACCURACY_VALUE',
'Maximum model space distance between geometric entities at asserted c
onnectivities');
#12736=UNCERTAINTY_MEASURE_WITH_UNIT(LENGTH_MEASURE(0.001),#12780,
'DISTANCE_ACCURACY_VALUE',
'Maximum model space distance between geometric entities at asserted c
onnectivities');
#12737=UNCERTAINTY_MEASURE_WITH_UNIT(LENGTH_MEASURE(0.001),#12780,
'DISTANCE_ACCURACY_VALUE',
'Maximum model space distance between geometric entities at asserted c
onnectivities');
#12738=UNCERTAINTY_MEASURE_WITH_UNIT(LENGTH_MEASURE(0.001),#12780,
'DISTANCE_ACCURACY_VALUE',
'Maximum model space distance between geometric entities at asserted c
onnectivities');
#12739=UNCERTAINTY_MEASURE_WITH_UNIT(LENGTH_MEASURE(0.001),#12780,
'DISTANCE_ACCURACY_VALUE',
'Maximum model space distance between geometric entities at asserted c
onnectivities');
#12740=(
GEOMETRIC_REPRESENTATION_CONTEXT(3)
GLOBAL_UNCERTAINTY_ASSIGNED_CONTEXT((#12700))
GLOBAL_UNIT_ASSIGNED_CONTEXT((#12780,#12782,#12783))
REPRESENTATION_CONTEXT('','3D')
);
#12741=(
GEOMETRIC_REPRESENTATION_CONTEXT(3)
GLOBAL_UNCERTAINTY_ASSIGNED_CONTEXT((#12701))
GLOBAL_UNIT_ASSIGNED_CONTEXT((#12780,#12782,#12783))
REPRESENTATION_CONTEXT('','3D')
);
#12742=(
GEOMETRIC_REPRESENTATION_CONTEXT(3)
GLOBAL_UNCERTAINTY_ASSIGNED_CONTEXT((#12702))
GLOBAL_UNIT_ASSIGNED_CONTEXT((#12780,#12782,#12783))
REPRESENTATION_CONTEXT('','3D')
);
#12743=(
GEOMETRIC_REPRESENTATION_CONTEXT(3)
GLOBAL_UNCERTAINTY_ASSIGNED_CONTEXT((#12703))
GLOBAL_UNIT_ASSIGNED_CONTEXT((#12780,#12782,#12783))
REPRESENTATION_CONTEXT('','3D')
);
#12744=(
GEOMETRIC_REPRESENTATION_CONTEXT(3)
GLOBAL_UNCERTAINTY_ASSIGNED_CONTEXT((#12704))
GLOBAL_UNIT_ASSIGNED_CONTEXT((#12780,#12782,#12783))
REPRESENTATION_CONTEXT('','3D')
);
#12745=(
GEOMETRIC_REPRESENTATION_CONTEXT(3)
GLOBAL_UNCERTAINTY_ASSIGNED_CONTEXT((#12705))
GLOBAL_UNIT_ASSIGNED_CONTEXT((#12780,#12782,#12783))
REPRESENTATION_CONTEXT('','3D')
);
#12746=(
GEOMETRIC_REPRESENTATION_CONTEXT(3)
GLOBAL_UNCERTAINTY_ASSIGNED_CONTEXT((#12706))
GLOBAL_UNIT_ASSIGNED_CONTEXT((#12780,#12782,#12783))
REPRESENTATION_CONTEXT('','3D')
);
#12747=(
GEOMETRIC_REPRESENTATION_CONTEXT(3)
GLOBAL_UNCERTAINTY_ASSIGNED_CONTEXT((#12707))
GLOBAL_UNIT_ASSIGNED_CONTEXT((#12780,#12782,#12783))
REPRESENTATION_CONTEXT('','3D')
);
#12748=(
GEOMETRIC_REPRESENTATION_CONTEXT(3)
GLOBAL_UNCERTAINTY_ASSIGNED_CONTEXT((#12708))
GLOBAL_UNIT_ASSIGNED_CONTEXT((#12780,#12782,#12783))
REPRESENTATION_CONTEXT('','3D')
);
#12749=(
GEOMETRIC_REPRESENTATION_CONTEXT(3)
GLOBAL_UNCERTAINTY_ASSIGNED_CONTEXT((#12709))
GLOBAL_UNIT_ASSIGNED_CONTEXT((#12780,#12782,#12783))
REPRESENTATION_CONTEXT('','3D')
);
#12750=(
GEOMETRIC_REPRESENTATION_CONTEXT(3)
GLOBAL_UNCERTAINTY_ASSIGNED_CONTEXT((#12710))
GLOBAL_UNIT_ASSIGNED_CONTEXT((#12780,#12782,#12783))
REPRESENTATION_CONTEXT('','3D')
);
#12751=(
GEOMETRIC_REPRESENTATION_CONTEXT(3)
GLOBAL_UNCERTAINTY_ASSIGNED_CONTEXT((#12711))
GLOBAL_UNIT_ASSIGNED_CONTEXT((#12780,#12782,#12783))
REPRESENTATION_CONTEXT('','3D')
);
#12752=(
GEOMETRIC_REPRESENTATION_CONTEXT(3)
GLOBAL_UNCERTAINTY_ASSIGNED_CONTEXT((#12712))
GLOBAL_UNIT_ASSIGNED_CONTEXT((#12780,#12782,#12783))
REPRESENTATION_CONTEXT('','3D')
);
#12753=(
GEOMETRIC_REPRESENTATION_CONTEXT(3)
GLOBAL_UNCERTAINTY_ASSIGNED_CONTEXT((#12713))
GLOBAL_UNIT_ASSIGNED_CONTEXT((#12780,#12782,#12783))
REPRESENTATION_CONTEXT('','3D')
);
#12754=(
GEOMETRIC_REPRESENTATION_CONTEXT(3)
GLOBAL_UNCERTAINTY_ASSIGNED_CONTEXT((#12714))
GLOBAL_UNIT_ASSIGNED_CONTEXT((#12780,#12782,#12783))
REPRESENTATION_CONTEXT('','3D')
);
#12755=(
GEOMETRIC_REPRESENTATION_CONTEXT(3)
GLOBAL_UNCERTAINTY_ASSIGNED_CONTEXT((#12715))
GLOBAL_UNIT_ASSIGNED_CONTEXT((#12780,#12782,#12783))
REPRESENTATION_CONTEXT('','3D')
);
#12756=(
GEOMETRIC_REPRESENTATION_CONTEXT(3)
GLOBAL_UNCERTAINTY_ASSIGNED_CONTEXT((#12716))
GLOBAL_UNIT_ASSIGNED_CONTEXT((#12780,#12782,#12783))
REPRESENTATION_CONTEXT('','3D')
);
#12757=(
GEOMETRIC_REPRESENTATION_CONTEXT(3)
GLOBAL_UNCERTAINTY_ASSIGNED_CONTEXT((#12717))
GLOBAL_UNIT_ASSIGNED_CONTEXT((#12780,#12782,#12783))
REPRESENTATION_CONTEXT('','3D')
);
#12758=(
GEOMETRIC_REPRESENTATION_CONTEXT(3)
GLOBAL_UNCERTAINTY_ASSIGNED_CONTEXT((#12718))
GLOBAL_UNIT_ASSIGNED_CONTEXT((#12780,#12782,#12783))
REPRESENTATION_CONTEXT('','3D')
);
#12759=(
GEOMETRIC_REPRESENTATION_CONTEXT(3)
GLOBAL_UNCERTAINTY_ASSIGNED_CONTEXT((#12719))
GLOBAL_UNIT_ASSIGNED_CONTEXT((#12780,#12782,#12783))
REPRESENTATION_CONTEXT('','3D')
);
#12760=(
GEOMETRIC_REPRESENTATION_CONTEXT(3)
GLOBAL_UNCERTAINTY_ASSIGNED_CONTEXT((#12720))
GLOBAL_UNIT_ASSIGNED_CONTEXT((#12780,#12782,#12783))
REPRESENTATION_CONTEXT('','3D')
);
#12761=(
GEOMETRIC_REPRESENTATION_CONTEXT(3)
GLOBAL_UNCERTAINTY_ASSIGNED_CONTEXT((#12721))
GLOBAL_UNIT_ASSIGNED_CONTEXT((#12780,#12782,#12783))
REPRESENTATION_CONTEXT('','3D')
);
#12762=(
GEOMETRIC_REPRESENTATION_CONTEXT(3)
GLOBAL_UNCERTAINTY_ASSIGNED_CONTEXT((#12722))
GLOBAL_UNIT_ASSIGNED_CONTEXT((#12780,#12782,#12783))
REPRESENTATION_CONTEXT('','3D')
);
#12763=(
GEOMETRIC_REPRESENTATION_CONTEXT(3)
GLOBAL_UNCERTAINTY_ASSIGNED_CONTEXT((#12723))
GLOBAL_UNIT_ASSIGNED_CONTEXT((#12780,#12782,#12783))
REPRESENTATION_CONTEXT('','3D')
);
#12764=(
GEOMETRIC_REPRESENTATION_CONTEXT(3)
GLOBAL_UNCERTAINTY_ASSIGNED_CONTEXT((#12724))
GLOBAL_UNIT_ASSIGNED_CONTEXT((#12780,#12782,#12783))
REPRESENTATION_CONTEXT('','3D')
);
#12765=(
GEOMETRIC_REPRESENTATION_CONTEXT(3)
GLOBAL_UNCERTAINTY_ASSIGNED_CONTEXT((#12725))
GLOBAL_UNIT_ASSIGNED_CONTEXT((#12780,#12782,#12783))
REPRESENTATION_CONTEXT('','3D')
);
#12766=(
GEOMETRIC_REPRESENTATION_CONTEXT(3)
GLOBAL_UNCERTAINTY_ASSIGNED_CONTEXT((#12726))
GLOBAL_UNIT_ASSIGNED_CONTEXT((#12780,#12782,#12783))
REPRESENTATION_CONTEXT('','3D')
);
#12767=(
GEOMETRIC_REPRESENTATION_CONTEXT(3)
GLOBAL_UNCERTAINTY_ASSIGNED_CONTEXT((#12727))
GLOBAL_UNIT_ASSIGNED_CONTEXT((#12780,#12782,#12783))
REPRESENTATION_CONTEXT('','3D')
);
#12768=(
GEOMETRIC_REPRESENTATION_CONTEXT(3)
GLOBAL_UNCERTAINTY_ASSIGNED_CONTEXT((#12728))
GLOBAL_UNIT_ASSIGNED_CONTEXT((#12780,#12782,#12783))
REPRESENTATION_CONTEXT('','3D')
);
#12769=(
GEOMETRIC_REPRESENTATION_CONTEXT(3)
GLOBAL_UNCERTAINTY_ASSIGNED_CONTEXT((#12729))
GLOBAL_UNIT_ASSIGNED_CONTEXT((#12780,#12782,#12783))
REPRESENTATION_CONTEXT('','3D')
);
#12770=(
GEOMETRIC_REPRESENTATION_CONTEXT(3)
GLOBAL_UNCERTAINTY_ASSIGNED_CONTEXT((#12730))
GLOBAL_UNIT_ASSIGNED_CONTEXT((#12780,#12782,#12783))
REPRESENTATION_CONTEXT('','3D')
);
#12771=(
GEOMETRIC_REPRESENTATION_CONTEXT(3)
GLOBAL_UNCERTAINTY_ASSIGNED_CONTEXT((#12731))
GLOBAL_UNIT_ASSIGNED_CONTEXT((#12780,#12782,#12783))
REPRESENTATION_CONTEXT('','3D')
);
#12772=(
GEOMETRIC_REPRESENTATION_CONTEXT(3)
GLOBAL_UNCERTAINTY_ASSIGNED_CONTEXT((#12732))
GLOBAL_UNIT_ASSIGNED_CONTEXT((#12780,#12782,#12783))
REPRESENTATION_CONTEXT('','3D')
);
#12773=(
GEOMETRIC_REPRESENTATION_CONTEXT(3)
GLOBAL_UNCERTAINTY_ASSIGNED_CONTEXT((#12733))
GLOBAL_UNIT_ASSIGNED_CONTEXT((#12780,#12782,#12783))
REPRESENTATION_CONTEXT('','3D')
);
#12774=(
GEOMETRIC_REPRESENTATION_CONTEXT(3)
GLOBAL_UNCERTAINTY_ASSIGNED_CONTEXT((#12734))
GLOBAL_UNIT_ASSIGNED_CONTEXT((#12780,#12782,#12783))
REPRESENTATION_CONTEXT('','3D')
);
#12775=(
GEOMETRIC_REPRESENTATION_CONTEXT(3)
GLOBAL_UNCERTAINTY_ASSIGNED_CONTEXT((#12735))
GLOBAL_UNIT_ASSIGNED_CONTEXT((#12780,#12782,#12783))
REPRESENTATION_CONTEXT('','3D')
);
#12776=(
GEOMETRIC_REPRESENTATION_CONTEXT(3)
GLOBAL_UNCERTAINTY_ASSIGNED_CONTEXT((#12736))
GLOBAL_UNIT_ASSIGNED_CONTEXT((#12780,#12782,#12783))
REPRESENTATION_CONTEXT('','3D')
);
#12777=(
GEOMETRIC_REPRESENTATION_CONTEXT(3)
GLOBAL_UNCERTAINTY_ASSIGNED_CONTEXT((#12737))
GLOBAL_UNIT_ASSIGNED_CONTEXT((#12780,#12782,#12783))
REPRESENTATION_CONTEXT('','3D')
);
#12778=(
GEOMETRIC_REPRESENTATION_CONTEXT(3)
GLOBAL_UNCERTAINTY_ASSIGNED_CONTEXT((#12738))
GLOBAL_UNIT_ASSIGNED_CONTEXT((#12780,#12782,#12783))
REPRESENTATION_CONTEXT('','3D')
);
#12779=(
GEOMETRIC_REPRESENTATION_CONTEXT(3)
GLOBAL_UNCERTAINTY_ASSIGNED_CONTEXT((#12739))
GLOBAL_UNIT_ASSIGNED_CONTEXT((#12780,#12782,#12783))
REPRESENTATION_CONTEXT('','3D')
);
#12780=(
LENGTH_UNIT()
NAMED_UNIT(*)
SI_UNIT(.CENTI.,.METRE.)
);
#12781=(
LENGTH_UNIT()
NAMED_UNIT(*)
SI_UNIT($,.METRE.)
);
#12782=(
NAMED_UNIT(*)
PLANE_ANGLE_UNIT()
SI_UNIT($,.RADIAN.)
);
#12783=(
NAMED_UNIT(*)
SI_UNIT($,.STERADIAN.)
SOLID_ANGLE_UNIT()
);
#12784=SHAPE_DEFINITION_REPRESENTATION(#12823,#12923);
#12785=SHAPE_DEFINITION_REPRESENTATION(#12824,#12924);
#12786=SHAPE_DEFINITION_REPRESENTATION(#12825,#12925);
#12787=SHAPE_DEFINITION_REPRESENTATION(#12826,#12926);
#12788=SHAPE_DEFINITION_REPRESENTATION(#12827,#12927);
#12789=SHAPE_DEFINITION_REPRESENTATION(#12828,#12928);
#12790=SHAPE_DEFINITION_REPRESENTATION(#12829,#12929);
#12791=SHAPE_DEFINITION_REPRESENTATION(#12830,#12930);
#12792=SHAPE_DEFINITION_REPRESENTATION(#12831,#12931);
#12793=SHAPE_DEFINITION_REPRESENTATION(#12832,#12932);
#12794=SHAPE_DEFINITION_REPRESENTATION(#12833,#12933);
#12795=SHAPE_DEFINITION_REPRESENTATION(#12834,#12934);
#12796=SHAPE_DEFINITION_REPRESENTATION(#12835,#12935);
#12797=SHAPE_DEFINITION_REPRESENTATION(#12836,#12936);
#12798=SHAPE_DEFINITION_REPRESENTATION(#12837,#12937);
#12799=SHAPE_DEFINITION_REPRESENTATION(#12838,#12938);
#12800=SHAPE_DEFINITION_REPRESENTATION(#12839,#12939);
#12801=SHAPE_DEFINITION_REPRESENTATION(#12840,#12940);
#12802=SHAPE_DEFINITION_REPRESENTATION(#12841,#12941);
#12803=SHAPE_DEFINITION_REPRESENTATION(#12842,#12942);
#12804=SHAPE_DEFINITION_REPRESENTATION(#12843,#12943);
#12805=SHAPE_DEFINITION_REPRESENTATION(#12844,#12944);
#12806=SHAPE_DEFINITION_REPRESENTATION(#12845,#12945);
#12807=SHAPE_DEFINITION_REPRESENTATION(#12846,#12946);
#12808=SHAPE_DEFINITION_REPRESENTATION(#12847,#12947);
#12809=SHAPE_DEFINITION_REPRESENTATION(#12848,#12948);
#12810=SHAPE_DEFINITION_REPRESENTATION(#12849,#12949);
#12811=SHAPE_DEFINITION_REPRESENTATION(#12855,#12950);
#12812=SHAPE_DEFINITION_REPRESENTATION(#12880,#12951);
#12813=SHAPE_DEFINITION_REPRESENTATION(#12881,#12952);
#12814=SHAPE_DEFINITION_REPRESENTATION(#12882,#12953);
#12815=SHAPE_DEFINITION_REPRESENTATION(#12883,#12954);
#12816=SHAPE_DEFINITION_REPRESENTATION(#12884,#12955);
#12817=SHAPE_DEFINITION_REPRESENTATION(#12885,#12956);
#12818=SHAPE_DEFINITION_REPRESENTATION(#12886,#12957);
#12819=SHAPE_DEFINITION_REPRESENTATION(#12887,#12958);
#12820=SHAPE_DEFINITION_REPRESENTATION(#12888,#12959);
#12821=SHAPE_DEFINITION_REPRESENTATION(#12908,#12960);
#12822=SHAPE_DEFINITION_REPRESENTATION(#12909,#12961);
#12823=PRODUCT_DEFINITION_SHAPE('',$,#12963);
#12824=PRODUCT_DEFINITION_SHAPE('',$,#12964);
#12825=PRODUCT_DEFINITION_SHAPE('',$,#12965);
#12826=PRODUCT_DEFINITION_SHAPE('',$,#12966);
#12827=PRODUCT_DEFINITION_SHAPE('',$,#12967);
#12828=PRODUCT_DEFINITION_SHAPE('',$,#12968);
#12829=PRODUCT_DEFINITION_SHAPE('',$,#12969);
#12830=PRODUCT_DEFINITION_SHAPE('',$,#12970);
#12831=PRODUCT_DEFINITION_SHAPE('',$,#12971);
#12832=PRODUCT_DEFINITION_SHAPE('',$,#12972);
#12833=PRODUCT_DEFINITION_SHAPE('',$,#12973);
#12834=PRODUCT_DEFINITION_SHAPE('',$,#12974);
#12835=PRODUCT_DEFINITION_SHAPE('',$,#12975);
#12836=PRODUCT_DEFINITION_SHAPE('',$,#12976);
#12837=PRODUCT_DEFINITION_SHAPE('',$,#12977);
#12838=PRODUCT_DEFINITION_SHAPE('',$,#12978);
#12839=PRODUCT_DEFINITION_SHAPE('',$,#12979);
#12840=PRODUCT_DEFINITION_SHAPE('',$,#12980);
#12841=PRODUCT_DEFINITION_SHAPE('',$,#12981);
#12842=PRODUCT_DEFINITION_SHAPE('',$,#12982);
#12843=PRODUCT_DEFINITION_SHAPE('',$,#12983);
#12844=PRODUCT_DEFINITION_SHAPE('',$,#12984);
#12845=PRODUCT_DEFINITION_SHAPE('',$,#12985);
#12846=PRODUCT_DEFINITION_SHAPE('',$,#12986);
#12847=PRODUCT_DEFINITION_SHAPE('',$,#12987);
#12848=PRODUCT_DEFINITION_SHAPE('',$,#12988);
#12849=PRODUCT_DEFINITION_SHAPE('',$,#12989);
#12850=PRODUCT_DEFINITION_SHAPE($,$,#194);
#12851=PRODUCT_DEFINITION_SHAPE($,$,#195);
#12852=PRODUCT_DEFINITION_SHAPE($,$,#196);
#12853=PRODUCT_DEFINITION_SHAPE($,$,#197);
#12854=PRODUCT_DEFINITION_SHAPE($,$,#198);
#12855=PRODUCT_DEFINITION_SHAPE('',$,#12990);
#12856=PRODUCT_DEFINITION_SHAPE($,$,#199);
#12857=PRODUCT_DEFINITION_SHAPE($,$,#200);
#12858=PRODUCT_DEFINITION_SHAPE($,$,#201);
#12859=PRODUCT_DEFINITION_SHAPE($,$,#202);
#12860=PRODUCT_DEFINITION_SHAPE($,$,#203);
#12861=PRODUCT_DEFINITION_SHAPE($,$,#204);
#12862=PRODUCT_DEFINITION_SHAPE($,$,#205);
#12863=PRODUCT_DEFINITION_SHAPE($,$,#206);
#12864=PRODUCT_DEFINITION_SHAPE($,$,#207);
#12865=PRODUCT_DEFINITION_SHAPE($,$,#208);
#12866=PRODUCT_DEFINITION_SHAPE($,$,#209);
#12867=PRODUCT_DEFINITION_SHAPE($,$,#210);
#12868=PRODUCT_DEFINITION_SHAPE($,$,#211);
#12869=PRODUCT_DEFINITION_SHAPE($,$,#212);
#12870=PRODUCT_DEFINITION_SHAPE($,$,#213);
#12871=PRODUCT_DEFINITION_SHAPE($,$,#214);
#12872=PRODUCT_DEFINITION_SHAPE($,$,#215);
#12873=PRODUCT_DEFINITION_SHAPE($,$,#216);
#12874=PRODUCT_DEFINITION_SHAPE($,$,#217);
#12875=PRODUCT_DEFINITION_SHAPE($,$,#218);
#12876=PRODUCT_DEFINITION_SHAPE($,$,#219);
#12877=PRODUCT_DEFINITION_SHAPE($,$,#220);
#12878=PRODUCT_DEFINITION_SHAPE($,$,#221);
#12879=PRODUCT_DEFINITION_SHAPE($,$,#222);
#12880=PRODUCT_DEFINITION_SHAPE('',$,#12991);
#12881=PRODUCT_DEFINITION_SHAPE('',$,#12992);
#12882=PRODUCT_DEFINITION_SHAPE('',$,#12993);
#12883=PRODUCT_DEFINITION_SHAPE('',$,#12994);
#12884=PRODUCT_DEFINITION_SHAPE('',$,#12995);
#12885=PRODUCT_DEFINITION_SHAPE('',$,#12996);
#12886=PRODUCT_DEFINITION_SHAPE('',$,#12997);
#12887=PRODUCT_DEFINITION_SHAPE('',$,#12998);
#12888=PRODUCT_DEFINITION_SHAPE('',$,#12999);
#12889=PRODUCT_DEFINITION_SHAPE($,$,#223);
#12890=PRODUCT_DEFINITION_SHAPE($,$,#224);
#12891=PRODUCT_DEFINITION_SHAPE($,$,#225);
#12892=PRODUCT_DEFINITION_SHAPE($,$,#226);
#12893=PRODUCT_DEFINITION_SHAPE($,$,#227);
#12894=PRODUCT_DEFINITION_SHAPE($,$,#228);
#12895=PRODUCT_DEFINITION_SHAPE($,$,#229);
#12896=PRODUCT_DEFINITION_SHAPE($,$,#230);
#12897=PRODUCT_DEFINITION_SHAPE($,$,#231);
#12898=PRODUCT_DEFINITION_SHAPE($,$,#232);
#12899=PRODUCT_DEFINITION_SHAPE($,$,#233);
#12900=PRODUCT_DEFINITION_SHAPE($,$,#234);
#12901=PRODUCT_DEFINITION_SHAPE($,$,#235);
#12902=PRODUCT_DEFINITION_SHAPE($,$,#236);
#12903=PRODUCT_DEFINITION_SHAPE($,$,#237);
#12904=PRODUCT_DEFINITION_SHAPE($,$,#238);
#12905=PRODUCT_DEFINITION_SHAPE($,$,#239);
#12906=PRODUCT_DEFINITION_SHAPE($,$,#240);
#12907=PRODUCT_DEFINITION_SHAPE($,$,#241);
#12908=PRODUCT_DEFINITION_SHAPE('',$,#13000);
#12909=PRODUCT_DEFINITION_SHAPE('',$,#13001);
#12910=PRODUCT_DEFINITION_SHAPE($,$,#242);
#12911=PRODUCT_DEFINITION_SHAPE($,$,#243);
#12912=PRODUCT_DEFINITION_SHAPE($,$,#244);
#12913=PRODUCT_DEFINITION_SHAPE($,$,#245);
#12914=PRODUCT_DEFINITION_SHAPE($,$,#246);
#12915=PRODUCT_DEFINITION_SHAPE($,$,#247);
#12916=PRODUCT_DEFINITION_SHAPE($,$,#248);
#12917=PRODUCT_DEFINITION_SHAPE($,$,#249);
#12918=PRODUCT_DEFINITION_SHAPE($,$,#250);
#12919=PRODUCT_DEFINITION_SHAPE($,$,#251);
#12920=PRODUCT_DEFINITION_SHAPE($,$,#252);
#12921=PRODUCT_DEFINITION_SHAPE($,$,#253);
#12922=PRODUCT_DEFINITION_SHAPE($,$,#254);
#12923=SHAPE_REPRESENTATION('',(#6602,#7430,#7431,#7432),#12740);
#12924=SHAPE_REPRESENTATION('',(#6603,#7235,#7236,#7237,#7238,#7239,#7240,
#7241,#7242,#7243,#7244,#7245,#7246,#7247,#7248,#7249,#7250,#7251,#7252,
#7253),#12741);
#12925=SHAPE_REPRESENTATION('',(#6604),#12742);
#12926=SHAPE_REPRESENTATION('',(#6626),#12743);
#12927=SHAPE_REPRESENTATION('',(#6633),#12744);
#12928=SHAPE_REPRESENTATION('',(#6640),#12745);
#12929=SHAPE_REPRESENTATION('',(#6667),#12746);
#12930=SHAPE_REPRESENTATION('',(#6681),#12747);
#12931=SHAPE_REPRESENTATION('',(#6692),#12748);
#12932=SHAPE_REPRESENTATION('',(#6715),#12749);
#12933=SHAPE_REPRESENTATION('',(#6729),#12750);
#12934=SHAPE_REPRESENTATION('',(#6740),#12751);
#12935=SHAPE_REPRESENTATION('',(#6766),#12752);
#12936=SHAPE_REPRESENTATION('',(#6782),#12753);
#12937=SHAPE_REPRESENTATION('',(#6808,#7124,#7125,#7126,#7127,#7128,#7129,
#7130,#7131,#7132,#7133,#7134,#7135,#7136,#7137,#7138,#7139,#7140,#7141,
#7142,#7143,#7144,#7145,#7146,#7147),#12754);
#12938=SHAPE_REPRESENTATION('',(#6809),#12755);
#12939=SHAPE_REPRESENTATION('',(#6850),#12756);
#12940=SHAPE_REPRESENTATION('',(#6875),#12757);
#12941=SHAPE_REPRESENTATION('',(#6900),#12758);
#12942=SHAPE_REPRESENTATION('',(#6925),#12759);
#12943=SHAPE_REPRESENTATION('',(#6950),#12760);
#12944=SHAPE_REPRESENTATION('',(#6966,#7095,#7096,#7097,#7098,#7099),#12761);
#12945=SHAPE_REPRESENTATION('',(#6967),#12762);
#12946=SHAPE_REPRESENTATION('',(#6987),#12763);
#12947=SHAPE_REPRESENTATION('',(#7007),#12764);
#12948=SHAPE_REPRESENTATION('',(#7024),#12765);
#12949=SHAPE_REPRESENTATION('',(#7078),#12766);
#12950=SHAPE_REPRESENTATION('',(#7100),#12767);
#12951=SHAPE_REPRESENTATION('',(#7148,#7420,#7421,#7422,#7423,#7424,#7425,
#7426,#7427,#7428,#7429),#12768);
#12952=SHAPE_REPRESENTATION('',(#7149),#12769);
#12953=SHAPE_REPRESENTATION('',(#7167),#12770);
#12954=SHAPE_REPRESENTATION('',(#7181),#12771);
#12955=SHAPE_REPRESENTATION('',(#7190),#12772);
#12956=SHAPE_REPRESENTATION('',(#7199),#12773);
#12957=SHAPE_REPRESENTATION('',(#7205),#12774);
#12958=SHAPE_REPRESENTATION('',(#7211),#12775);
#12959=SHAPE_REPRESENTATION('',(#7220),#12776);
#12960=SHAPE_REPRESENTATION('',(#7254),#12777);
#12961=SHAPE_REPRESENTATION('',(#7396),#12778);
#12962=PRODUCT_DEFINITION_CONTEXT('part definition',#13081,'design');
#12963=PRODUCT_DEFINITION('PAT-012','PAT-012',#13002,
#12962);
#12964=PRODUCT_DEFINITION('Pivot frame and installed torsion spring',
'Pivot frame and installed torsion spring',#13003,#12962);
#12965=PRODUCT_DEFINITION('Base','Base',#13004,#12962);
#12966=PRODUCT_DEFINITION('Foot','Foot',#13005,#12962);
#12967=PRODUCT_DEFINITION('Foot (1)','Foot (1)',#13006,#12962);
#12968=PRODUCT_DEFINITION('Pivot pedestal and pin',
'Pivot pedestal and pin',#13007,#12962);
#12969=PRODUCT_DEFINITION('Pivot collar','Pivot collar',#13008,#12962);
#12970=PRODUCT_DEFINITION('Fixed spring post','Fixed spring post',#13009,
#12962);
#12971=PRODUCT_DEFINITION('Installed torsion spring',
'Installed torsion spring',#13010,#12962);
#12972=PRODUCT_DEFINITION('Stop screw bracket','Stop screw bracket',#13011,
#12962);
#12973=PRODUCT_DEFINITION('Flat Washer - M5','Flat Washer - M5',#13012,
#12962);
#12974=PRODUCT_DEFINITION('Cap Screw - M5x20','Cap Screw - M5x20',#13013,
#12962);
#12975=PRODUCT_DEFINITION('Hex Nut - M5','Hex Nut - M5',#13014,#12962);
#12976=PRODUCT_DEFINITION('Cap Screw - M4x16','Cap Screw - M4x16',#13015,
#12962);
#12977=PRODUCT_DEFINITION('Pivoting arm','Pivoting arm',#13016,#12962);
#12978=PRODUCT_DEFINITION('Tensioner arm','Tensioner arm',#13017,#12962);
#12979=PRODUCT_DEFINITION('Bearing cap','Bearing cap',#13018,#12962);
#12980=PRODUCT_DEFINITION('Bearing cap (1)','Bearing cap (1)',#13019,#12962);
#12981=PRODUCT_DEFINITION('Bearing cap (2)','Bearing cap (2)',#13020,#12962);
#12982=PRODUCT_DEFINITION('Bearing cap (3)','Bearing cap (3)',#13021,#12962);
#12983=PRODUCT_DEFINITION('Arm spring bracket','Arm spring bracket',#13022,
#12962);
#12984=PRODUCT_DEFINITION('Sealed Ball Bearing - 10 x 30 x 9 mm',
'Sealed Ball Bearing - 10 x 30 x 9 mm',#13023,#12962);
#12985=PRODUCT_DEFINITION('Inner ring','Inner ring',#13024,#12962);
#12986=PRODUCT_DEFINITION('Outer ring','Outer ring',#13025,#12962);
#12987=PRODUCT_DEFINITION('Balls','Balls',#13026,#12962);
#12988=PRODUCT_DEFINITION('Cage','Cage',#13027,#12962);
#12989=PRODUCT_DEFINITION('Seals 2RS','Seals 2RS',#13028,#12962);
#12990=PRODUCT_DEFINITION('M4x7 cap screw','M4x7 cap screw',#13029,#12962);
#12991=PRODUCT_DEFINITION('Bearing-mounted idler',
'Bearing-mounted idler',#13030,#12962);
#12992=PRODUCT_DEFINITION('Stepped idler axle','Stepped idler axle',#13031,
#12962);
#12993=PRODUCT_DEFINITION('Idler collar','Idler collar',#13032,#12962);
#12994=PRODUCT_DEFINITION('Lower pulley spacer','Lower pulley spacer',#13033,
#12962);
#12995=PRODUCT_DEFINITION('Upper pulley spacer','Upper pulley spacer',#13034,
#12962);
#12996=PRODUCT_DEFINITION('M3 pulley set screw','M3 pulley set screw',#13035,
#12962);
#12997=PRODUCT_DEFINITION('M3 pulley set screw (1)',
'M3 pulley set screw (1)',#13036,#12962);
#12998=PRODUCT_DEFINITION('Axle keeper','Axle keeper',#13037,#12962);
#12999=PRODUCT_DEFINITION('M4x4 collar screw','M4x4 collar screw',#13038,
#12962);
#13000=PRODUCT_DEFINITION(
'Timing Pulley - 2 mm Pitch, 20 Teeth, 8 mm Bore',
'Timing Pulley - 2 mm Pitch, 20 Teeth, 8 mm Bore',#13039,#12962);
#13001=PRODUCT_DEFINITION('M4x10 Cap Screw','M4x10 Cap Screw',#13040,#12962);
#13002=PRODUCT_DEFINITION_FORMATION('',$,#13083);
#13003=PRODUCT_DEFINITION_FORMATION('',$,#13084);
#13004=PRODUCT_DEFINITION_FORMATION('',$,#13085);
#13005=PRODUCT_DEFINITION_FORMATION('',$,#13086);
#13006=PRODUCT_DEFINITION_FORMATION('',$,#13087);
#13007=PRODUCT_DEFINITION_FORMATION('',$,#13088);
#13008=PRODUCT_DEFINITION_FORMATION('',$,#13089);
#13009=PRODUCT_DEFINITION_FORMATION('',$,#13090);
#13010=PRODUCT_DEFINITION_FORMATION('',$,#13091);
#13011=PRODUCT_DEFINITION_FORMATION('',$,#13092);
#13012=PRODUCT_DEFINITION_FORMATION('',$,#13093);
#13013=PRODUCT_DEFINITION_FORMATION('',$,#13094);
#13014=PRODUCT_DEFINITION_FORMATION('',$,#13095);
#13015=PRODUCT_DEFINITION_FORMATION('',$,#13096);
#13016=PRODUCT_DEFINITION_FORMATION('',$,#13097);
#13017=PRODUCT_DEFINITION_FORMATION('',$,#13098);
#13018=PRODUCT_DEFINITION_FORMATION('',$,#13099);
#13019=PRODUCT_DEFINITION_FORMATION('',$,#13100);
#13020=PRODUCT_DEFINITION_FORMATION('',$,#13101);
#13021=PRODUCT_DEFINITION_FORMATION('',$,#13102);
#13022=PRODUCT_DEFINITION_FORMATION('',$,#13103);
#13023=PRODUCT_DEFINITION_FORMATION('',$,#13104);
#13024=PRODUCT_DEFINITION_FORMATION('',$,#13105);
#13025=PRODUCT_DEFINITION_FORMATION('',$,#13106);
#13026=PRODUCT_DEFINITION_FORMATION('',$,#13107);
#13027=PRODUCT_DEFINITION_FORMATION('',$,#13108);
#13028=PRODUCT_DEFINITION_FORMATION('',$,#13109);
#13029=PRODUCT_DEFINITION_FORMATION('',$,#13110);
#13030=PRODUCT_DEFINITION_FORMATION('',$,#13111);
#13031=PRODUCT_DEFINITION_FORMATION('',$,#13112);
#13032=PRODUCT_DEFINITION_FORMATION('',$,#13113);
#13033=PRODUCT_DEFINITION_FORMATION('',$,#13114);
#13034=PRODUCT_DEFINITION_FORMATION('',$,#13115);
#13035=PRODUCT_DEFINITION_FORMATION('',$,#13116);
#13036=PRODUCT_DEFINITION_FORMATION('',$,#13117);
#13037=PRODUCT_DEFINITION_FORMATION('',$,#13118);
#13038=PRODUCT_DEFINITION_FORMATION('',$,#13119);
#13039=PRODUCT_DEFINITION_FORMATION('',$,#13120);
#13040=PRODUCT_DEFINITION_FORMATION('',$,#13121);
#13041=PRODUCT_RELATED_PRODUCT_CATEGORY('PAT-012','PAT-012',(#13083));
#13042=PRODUCT_RELATED_PRODUCT_CATEGORY(
'Pivot frame and installed torsion spring',
'Pivot frame and installed torsion spring',(#13084));
#13043=PRODUCT_RELATED_PRODUCT_CATEGORY('Base','Base',(#13085));
#13044=PRODUCT_RELATED_PRODUCT_CATEGORY('Foot','Foot',(#13086));
#13045=PRODUCT_RELATED_PRODUCT_CATEGORY('Foot (1)','Foot (1)',(#13087));
#13046=PRODUCT_RELATED_PRODUCT_CATEGORY('Pivot pedestal and pin',
'Pivot pedestal and pin',(#13088));
#13047=PRODUCT_RELATED_PRODUCT_CATEGORY('Pivot collar','Pivot collar',(#13089));
#13048=PRODUCT_RELATED_PRODUCT_CATEGORY('Fixed spring post',
'Fixed spring post',(#13090));
#13049=PRODUCT_RELATED_PRODUCT_CATEGORY('Installed torsion spring',
'Installed torsion spring',(#13091));
#13050=PRODUCT_RELATED_PRODUCT_CATEGORY('Stop screw bracket',
'Stop screw bracket',(#13092));
#13051=PRODUCT_RELATED_PRODUCT_CATEGORY('Flat Washer - M5',
'Flat Washer - M5',(#13093));
#13052=PRODUCT_RELATED_PRODUCT_CATEGORY('Cap Screw - M5x20',
'Cap Screw - M5x20',(#13094));
#13053=PRODUCT_RELATED_PRODUCT_CATEGORY('Hex Nut - M5','Hex Nut - M5',(#13095));
#13054=PRODUCT_RELATED_PRODUCT_CATEGORY('Cap Screw - M4x16',
'Cap Screw - M4x16',(#13096));
#13055=PRODUCT_RELATED_PRODUCT_CATEGORY('Pivoting arm','Pivoting arm',(#13097));
#13056=PRODUCT_RELATED_PRODUCT_CATEGORY('Tensioner arm','Tensioner arm',
(#13098));
#13057=PRODUCT_RELATED_PRODUCT_CATEGORY('Bearing cap','Bearing cap',(#13099));
#13058=PRODUCT_RELATED_PRODUCT_CATEGORY('Bearing cap (1)',
'Bearing cap (1)',(#13100));
#13059=PRODUCT_RELATED_PRODUCT_CATEGORY('Bearing cap (2)',
'Bearing cap (2)',(#13101));
#13060=PRODUCT_RELATED_PRODUCT_CATEGORY('Bearing cap (3)',
'Bearing cap (3)',(#13102));
#13061=PRODUCT_RELATED_PRODUCT_CATEGORY('Arm spring bracket',
'Arm spring bracket',(#13103));
#13062=PRODUCT_RELATED_PRODUCT_CATEGORY(
'Sealed Ball Bearing - 10 x 30 x 9 mm',
'Sealed Ball Bearing - 10 x 30 x 9 mm',(#13104));
#13063=PRODUCT_RELATED_PRODUCT_CATEGORY('Inner ring','Inner ring',(#13105));
#13064=PRODUCT_RELATED_PRODUCT_CATEGORY('Outer ring','Outer ring',(#13106));
#13065=PRODUCT_RELATED_PRODUCT_CATEGORY('Balls','Balls',(#13107));
#13066=PRODUCT_RELATED_PRODUCT_CATEGORY('Cage','Cage',(#13108));
#13067=PRODUCT_RELATED_PRODUCT_CATEGORY('Seals 2RS','Seals 2RS',(#13109));
#13068=PRODUCT_RELATED_PRODUCT_CATEGORY('M4x7 cap screw',
'M4x7 cap screw',(#13110));
#13069=PRODUCT_RELATED_PRODUCT_CATEGORY('Bearing-mounted idler',
'Bearing-mounted idler',(#13111));
#13070=PRODUCT_RELATED_PRODUCT_CATEGORY('Stepped idler axle',
'Stepped idler axle',(#13112));
#13071=PRODUCT_RELATED_PRODUCT_CATEGORY('Idler collar','Idler collar',(#13113));
#13072=PRODUCT_RELATED_PRODUCT_CATEGORY('Lower pulley spacer',
'Lower pulley spacer',(#13114));
#13073=PRODUCT_RELATED_PRODUCT_CATEGORY('Upper pulley spacer',
'Upper pulley spacer',(#13115));
#13074=PRODUCT_RELATED_PRODUCT_CATEGORY('M3 pulley set screw',
'M3 pulley set screw',(#13116));
#13075=PRODUCT_RELATED_PRODUCT_CATEGORY('M3 pulley set screw (1)',
'M3 pulley set screw (1)',(#13117));
#13076=PRODUCT_RELATED_PRODUCT_CATEGORY('Axle keeper','Axle keeper',(#13118));
#13077=PRODUCT_RELATED_PRODUCT_CATEGORY('M4x4 collar screw',
'M4x4 collar screw',(#13119));
#13078=PRODUCT_RELATED_PRODUCT_CATEGORY(
'Timing Pulley - 2 mm Pitch, 20 Teeth, 8 mm Bore',
'Timing Pulley - 2 mm Pitch, 20 Teeth, 8 mm Bore',(#13120));
#13079=PRODUCT_RELATED_PRODUCT_CATEGORY('M4x10 Cap Screw',
'M4x10 Cap Screw',(#13121));
#13080=APPLICATION_PROTOCOL_DEFINITION('international standard',
'automotive_design',2009,#13081);
#13081=APPLICATION_CONTEXT(
'Core Data for Automotive Mechanical Design Process');
#13082=PRODUCT_CONTEXT('part definition',#13081,'mechanical');
#13083=PRODUCT('PAT-012','PAT-012',
'PAT-012',(#13082));
#13084=PRODUCT('Pivot frame and installed torsion spring',
'Pivot frame and installed torsion spring',
'Pivot frame and installed torsion spring',(#13082));
#13085=PRODUCT('Base','Base','Base',(#13082));
#13086=PRODUCT('Foot','Foot','Foot',(#13082));
#13087=PRODUCT('Foot (1)','Foot (1)','Foot (1)',(#13082));
#13088=PRODUCT('Pivot pedestal and pin','Pivot pedestal and pin',
'Pivot pedestal and pin',(#13082));
#13089=PRODUCT('Pivot collar','Pivot collar','Pivot collar',(#13082));
#13090=PRODUCT('Fixed spring post','Fixed spring post',
'Fixed spring post',(#13082));
#13091=PRODUCT('Installed torsion spring','Installed torsion spring',
'Installed torsion spring',(#13082));
#13092=PRODUCT('Stop screw bracket','Stop screw bracket',
'Stop screw bracket',(#13082));
#13093=PRODUCT('Flat Washer - M5','Flat Washer - M5','Flat Washer - M5',
(#13082));
#13094=PRODUCT('Cap Screw - M5x20','Cap Screw - M5x20',
'Cap Screw - M5x20',(#13082));
#13095=PRODUCT('Hex Nut - M5','Hex Nut - M5','Hex Nut - M5',(#13082));
#13096=PRODUCT('Cap Screw - M4x16','Cap Screw - M4x16',
'Cap Screw - M4x16',(#13082));
#13097=PRODUCT('Pivoting arm','Pivoting arm','Pivoting arm',(#13082));
#13098=PRODUCT('Tensioner arm','Tensioner arm','Tensioner arm',(#13082));
#13099=PRODUCT('Bearing cap','Bearing cap','Bearing cap',(#13082));
#13100=PRODUCT('Bearing cap (1)','Bearing cap (1)','Bearing cap (1)',(#13082));
#13101=PRODUCT('Bearing cap (2)','Bearing cap (2)','Bearing cap (2)',(#13082));
#13102=PRODUCT('Bearing cap (3)','Bearing cap (3)','Bearing cap (3)',(#13082));
#13103=PRODUCT('Arm spring bracket','Arm spring bracket',
'Arm spring bracket',(#13082));
#13104=PRODUCT('Sealed Ball Bearing - 10 x 30 x 9 mm',
'Sealed Ball Bearing - 10 x 30 x 9 mm',
'Sealed Ball Bearing - 10 x 30 x 9 mm',(#13082));
#13105=PRODUCT('Inner ring','Inner ring','Inner ring',(#13082));
#13106=PRODUCT('Outer ring','Outer ring','Outer ring',(#13082));
#13107=PRODUCT('Balls','Balls','Balls',(#13082));
#13108=PRODUCT('Cage','Cage','Cage',(#13082));
#13109=PRODUCT('Seals 2RS','Seals 2RS','Seals 2RS',(#13082));
#13110=PRODUCT('M4x7 cap screw','M4x7 cap screw','M4x7 cap screw',(#13082));
#13111=PRODUCT('Bearing-mounted idler','Bearing-mounted idler',
'Bearing-mounted idler',(#13082));
#13112=PRODUCT('Stepped idler axle','Stepped idler axle',
'Stepped idler axle',(#13082));
#13113=PRODUCT('Idler collar','Idler collar','Idler collar',(#13082));
#13114=PRODUCT('Lower pulley spacer','Lower pulley spacer',
'Lower pulley spacer',(#13082));
#13115=PRODUCT('Upper pulley spacer','Upper pulley spacer',
'Upper pulley spacer',(#13082));
#13116=PRODUCT('M3 pulley set screw','M3 pulley set screw',
'M3 pulley set screw',(#13082));
#13117=PRODUCT('M3 pulley set screw (1)','M3 pulley set screw (1)',
'M3 pulley set screw (1)',(#13082));
#13118=PRODUCT('Axle keeper','Axle keeper','Axle keeper',(#13082));
#13119=PRODUCT('M4x4 collar screw','M4x4 collar screw',
'M4x4 collar screw',(#13082));
#13120=PRODUCT('Timing Pulley - 2 mm Pitch, 20 Teeth, 8 mm Bore',
'Timing Pulley - 2 mm Pitch, 20 Teeth, 8 mm Bore',
'Timing Pulley - 2 mm Pitch, 20 Teeth, 8 mm Bore',(#13082));
#13121=PRODUCT('M4x10 Cap Screw','M4x10 Cap Screw','M4x10 Cap Screw',(#13082));
#13122=PRESENTATION_STYLE_ASSIGNMENT((#13127));
#13123=PRESENTATION_STYLE_ASSIGNMENT((#13128));
#13124=PRESENTATION_STYLE_ASSIGNMENT((#13129));
#13125=PRESENTATION_STYLE_ASSIGNMENT((#13130));
#13126=PRESENTATION_STYLE_ASSIGNMENT((#13131));
#13127=SURFACE_STYLE_USAGE(.BOTH.,#13132);
#13128=SURFACE_STYLE_USAGE(.BOTH.,#13133);
#13129=SURFACE_STYLE_USAGE(.BOTH.,#13134);
#13130=SURFACE_STYLE_USAGE(.BOTH.,#13135);
#13131=SURFACE_STYLE_USAGE(.BOTH.,#13136);
#13132=SURFACE_SIDE_STYLE('',(#13137));
#13133=SURFACE_SIDE_STYLE('',(#13138));
#13134=SURFACE_SIDE_STYLE('',(#13139));
#13135=SURFACE_SIDE_STYLE('',(#13140));
#13136=SURFACE_SIDE_STYLE('',(#13141));
#13137=SURFACE_STYLE_FILL_AREA(#13142);
#13138=SURFACE_STYLE_FILL_AREA(#13143);
#13139=SURFACE_STYLE_FILL_AREA(#13144);
#13140=SURFACE_STYLE_FILL_AREA(#13145);
#13141=SURFACE_STYLE_FILL_AREA(#13146);
#13142=FILL_AREA_STYLE('Steel - Satin',(#13147));
#13143=FILL_AREA_STYLE('CAD Library Painted - Deep blue',(#13148));
#13144=FILL_AREA_STYLE('CAD Library Painted - Engineering blue',(#13149));
#13145=FILL_AREA_STYLE('CAD Library Painted - Steel gray',(#13150));
#13146=FILL_AREA_STYLE('CAD Library Painted - Graphite',(#13151));
#13147=FILL_AREA_STYLE_COLOUR('Steel - Satin',#13152);
#13148=FILL_AREA_STYLE_COLOUR('CAD Library Painted - Deep blue',#13153);
#13149=FILL_AREA_STYLE_COLOUR('CAD Library Painted - Engineering blue',
#13154);
#13150=FILL_AREA_STYLE_COLOUR('CAD Library Painted - Steel gray',#13155);
#13151=FILL_AREA_STYLE_COLOUR('CAD Library Painted - Graphite',#13156);
#13152=COLOUR_RGB('Steel - Satin',0.627450980392157,0.627450980392157,0.627450980392157);
#13153=COLOUR_RGB('CAD Library Painted - Deep blue',0.0784313725490196,
0.203921568627451,0.349019607843137);
#13154=COLOUR_RGB('CAD Library Painted - Engineering blue',0.12156862745098,
0.356862745098039,0.6);
#13155=COLOUR_RGB('CAD Library Painted - Steel gray',0.592156862745098,
0.631372549019608,0.67843137254902);
#13156=COLOUR_RGB('CAD Library Painted - Graphite',0.168627450980392,0.192156862745098,
0.231372549019608);
#13157=COLOUR_RGB('Dark Blue',0.08,0.2,0.34);
#13158=FILL_AREA_STYLE_COLOUR('',#13157);
#13159=FILL_AREA_STYLE('',(#13158));
#13160=SURFACE_STYLE_FILL_AREA(#13159);
#13161=SURFACE_SIDE_STYLE('',(#13160));
#13162=SURFACE_STYLE_USAGE(.BOTH.,#13161);
#13163=PRESENTATION_STYLE_ASSIGNMENT((#13162));
#13164=COLOUR_RGB('Light Blue',0.38,0.62,0.78);
#13165=FILL_AREA_STYLE_COLOUR('',#13164);
#13166=FILL_AREA_STYLE('',(#13165));
#13167=SURFACE_STYLE_FILL_AREA(#13166);
#13168=SURFACE_SIDE_STYLE('',(#13167));
#13169=SURFACE_STYLE_USAGE(.BOTH.,#13168);
#13170=PRESENTATION_STYLE_ASSIGNMENT((#13169));
#13171=COLOUR_RGB('Sky Blue',0.24,0.69,0.87);
#13172=FILL_AREA_STYLE_COLOUR('',#13171);
#13173=FILL_AREA_STYLE('',(#13172));
#13174=SURFACE_STYLE_FILL_AREA(#13173);
#13175=SURFACE_SIDE_STYLE('',(#13174));
#13176=SURFACE_STYLE_USAGE(.BOTH.,#13175);
#13177=PRESENTATION_STYLE_ASSIGNMENT((#13176));
#13178=COLOUR_RGB('Grey',0.48,0.52,0.57);
#13179=FILL_AREA_STYLE_COLOUR('',#13178);
#13180=FILL_AREA_STYLE('',(#13179));
#13181=SURFACE_STYLE_FILL_AREA(#13180);
#13182=SURFACE_SIDE_STYLE('',(#13181));
#13183=SURFACE_STYLE_USAGE(.BOTH.,#13182);
#13184=PRESENTATION_STYLE_ASSIGNMENT((#13183));
#13185=COLOUR_RGB('Black',0.12,0.14,0.17);
#13186=FILL_AREA_STYLE_COLOUR('',#13185);
#13187=FILL_AREA_STYLE('',(#13186));
#13188=SURFACE_STYLE_FILL_AREA(#13187);
#13189=SURFACE_SIDE_STYLE('',(#13188));
#13190=SURFACE_STYLE_USAGE(.BOTH.,#13189);
#13191=PRESENTATION_STYLE_ASSIGNMENT((#13190));
#13192=COLOUR_RGB('Off White',0.89,0.88,0.83);
#13193=FILL_AREA_STYLE_COLOUR('',#13192);
#13194=FILL_AREA_STYLE('',(#13193));
#13195=SURFACE_STYLE_FILL_AREA(#13194);
#13196=SURFACE_SIDE_STYLE('',(#13195));
#13197=SURFACE_STYLE_USAGE(.BOTH.,#13196);
#13198=PRESENTATION_STYLE_ASSIGNMENT((#13197));
ENDSEC;
END-ISO-10303-21;
